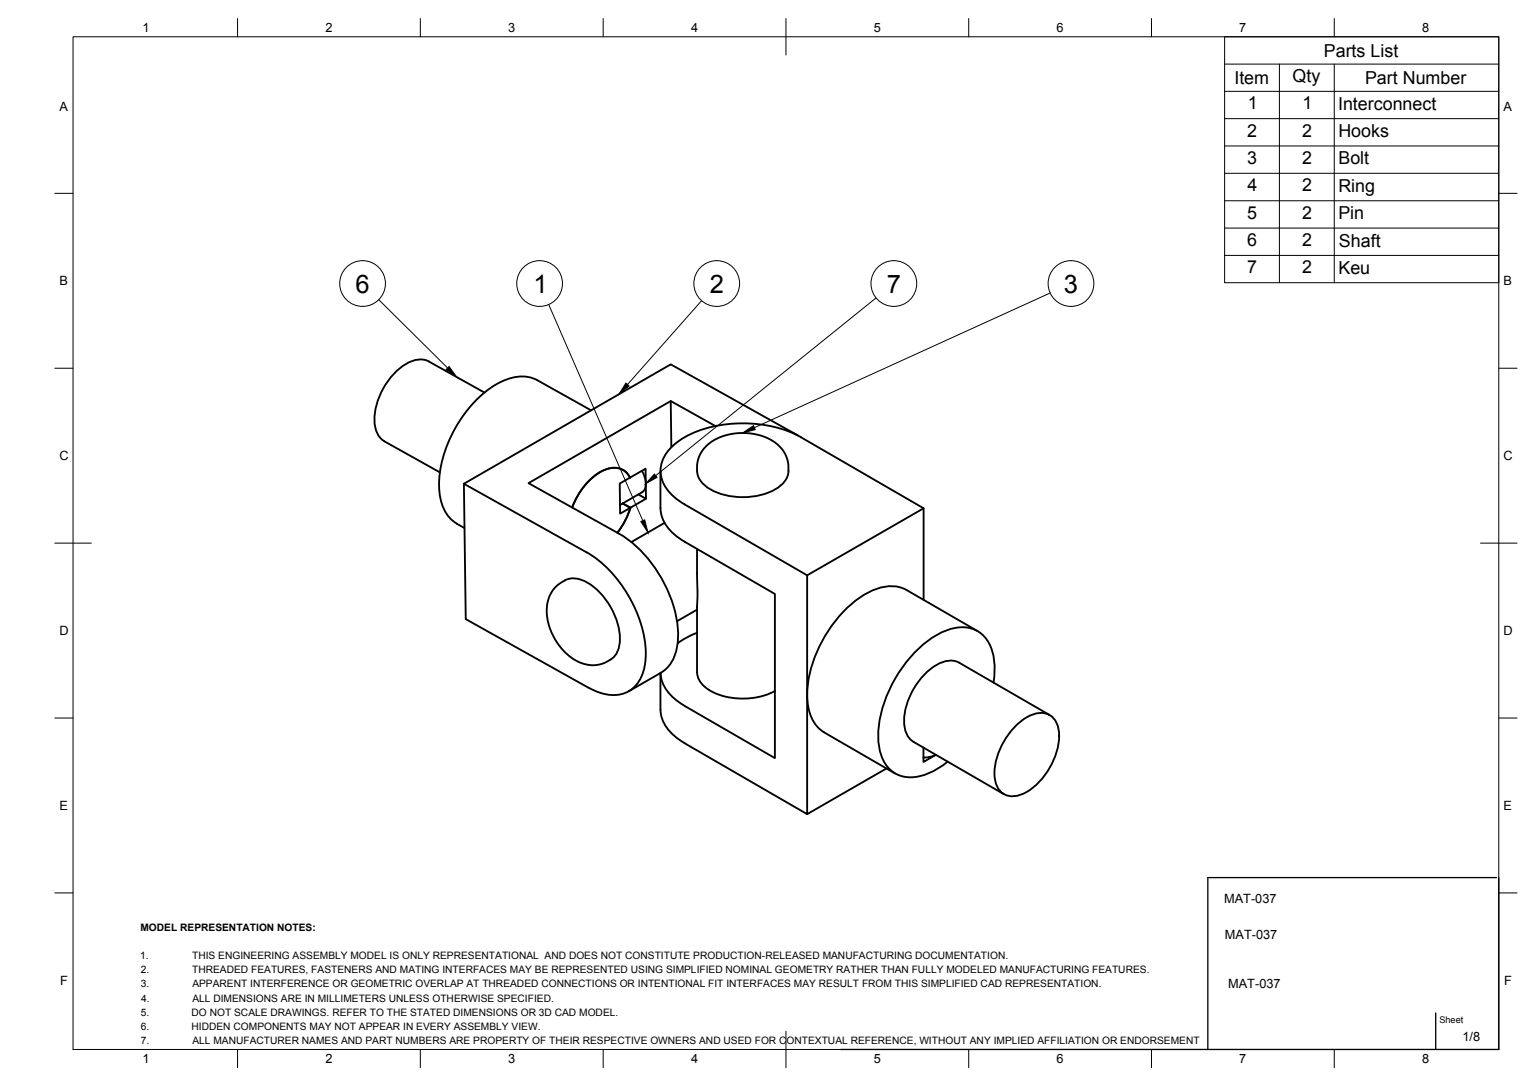
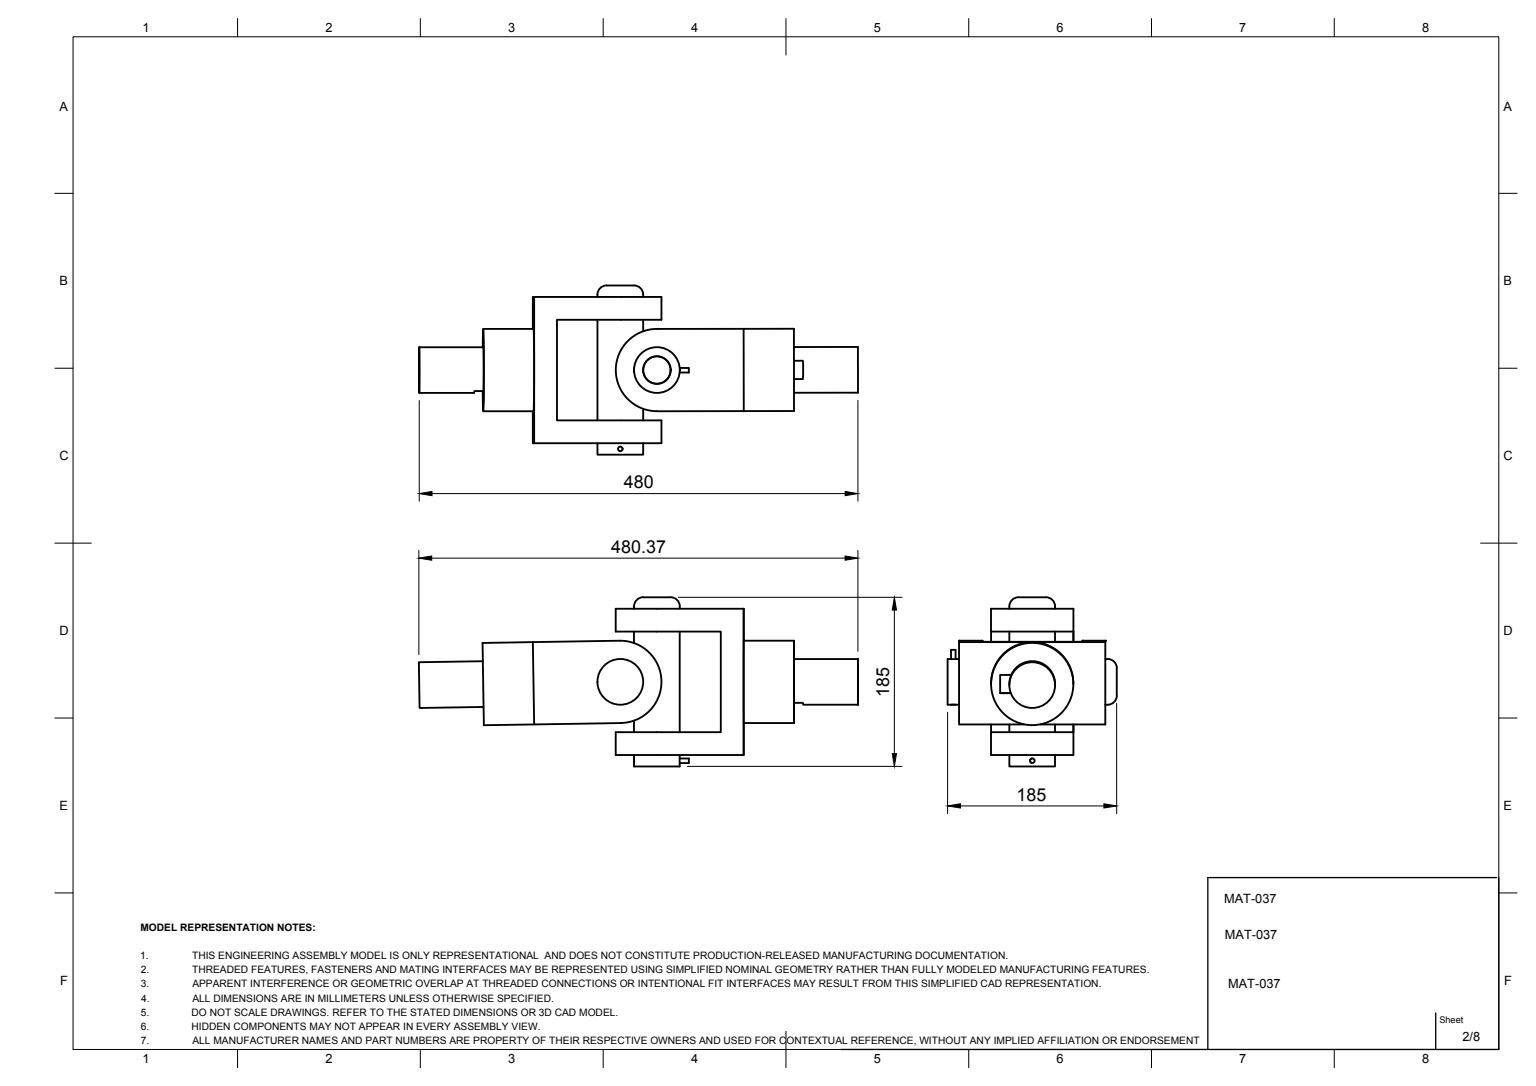
ISO-10303-21;
HEADER;
/* Generated by software containing ST-Developer
 * from STEP Tools, Inc. (www.steptools.com) 
 */

FILE_DESCRIPTION(
/* description */ ('STEP AP214'),
/* implementation_level */ '2;1');

FILE_NAME(
/* name */ 'MAT-037.step',
/* time_stamp */ '2026-11-14T21:09:07-08:00',
/* author */ (''),
/* organization */ (''),
/* preprocessor_version */ 'ST-DEVELOPER v20.2',
/* originating_system */ 'Autodesk Translation Framework v15.17.0.0',
/* authorisation */ '');

FILE_SCHEMA (('AUTOMOTIVE_DESIGN { 1 0 10303 214 3 1 1 }'));
ENDSEC;

DATA;
#10=MECHANICAL_DESIGN_GEOMETRIC_PRESENTATION_REPRESENTATION('',(#78,#79,
#80,#81,#82,#83,#84),#2059);
#11=ITEM_DEFINED_TRANSFORMATION($,$,#1061,#1167);
#12=ITEM_DEFINED_TRANSFORMATION($,$,#1078,#1168);
#13=ITEM_DEFINED_TRANSFORMATION($,$,#1111,#1169);
#14=ITEM_DEFINED_TRANSFORMATION($,$,#1126,#1170);
#15=ITEM_DEFINED_TRANSFORMATION($,$,#1137,#1171);
#16=ITEM_DEFINED_TRANSFORMATION($,$,#1143,#1172);
#17=ITEM_DEFINED_TRANSFORMATION($,$,#1156,#1173);
#18=ITEM_DEFINED_TRANSFORMATION($,$,#1078,#1174);
#19=ITEM_DEFINED_TRANSFORMATION($,$,#1111,#1175);
#20=ITEM_DEFINED_TRANSFORMATION($,$,#1126,#1176);
#21=ITEM_DEFINED_TRANSFORMATION($,$,#1137,#1177);
#22=ITEM_DEFINED_TRANSFORMATION($,$,#1143,#1178);
#23=ITEM_DEFINED_TRANSFORMATION($,$,#1156,#1179);
#24=(
REPRESENTATION_RELATIONSHIP($,$,#2094,#2093)
REPRESENTATION_RELATIONSHIP_WITH_TRANSFORMATION(#11)
SHAPE_REPRESENTATION_RELATIONSHIP()
);
#25=(
REPRESENTATION_RELATIONSHIP($,$,#2095,#2093)
REPRESENTATION_RELATIONSHIP_WITH_TRANSFORMATION(#12)
SHAPE_REPRESENTATION_RELATIONSHIP()
);
#26=(
REPRESENTATION_RELATIONSHIP($,$,#2096,#2093)
REPRESENTATION_RELATIONSHIP_WITH_TRANSFORMATION(#13)
SHAPE_REPRESENTATION_RELATIONSHIP()
);
#27=(
REPRESENTATION_RELATIONSHIP($,$,#2097,#2093)
REPRESENTATION_RELATIONSHIP_WITH_TRANSFORMATION(#14)
SHAPE_REPRESENTATION_RELATIONSHIP()
);
#28=(
REPRESENTATION_RELATIONSHIP($,$,#2098,#2093)
REPRESENTATION_RELATIONSHIP_WITH_TRANSFORMATION(#15)
SHAPE_REPRESENTATION_RELATIONSHIP()
);
#29=(
REPRESENTATION_RELATIONSHIP($,$,#2099,#2093)
REPRESENTATION_RELATIONSHIP_WITH_TRANSFORMATION(#16)
SHAPE_REPRESENTATION_RELATIONSHIP()
);
#30=(
REPRESENTATION_RELATIONSHIP($,$,#2100,#2093)
REPRESENTATION_RELATIONSHIP_WITH_TRANSFORMATION(#17)
SHAPE_REPRESENTATION_RELATIONSHIP()
);
#31=(
REPRESENTATION_RELATIONSHIP($,$,#2095,#2093)
REPRESENTATION_RELATIONSHIP_WITH_TRANSFORMATION(#18)
SHAPE_REPRESENTATION_RELATIONSHIP()
);
#32=(
REPRESENTATION_RELATIONSHIP($,$,#2096,#2093)
REPRESENTATION_RELATIONSHIP_WITH_TRANSFORMATION(#19)
SHAPE_REPRESENTATION_RELATIONSHIP()
);
#33=(
REPRESENTATION_RELATIONSHIP($,$,#2097,#2093)
REPRESENTATION_RELATIONSHIP_WITH_TRANSFORMATION(#20)
SHAPE_REPRESENTATION_RELATIONSHIP()
);
#34=(
REPRESENTATION_RELATIONSHIP($,$,#2098,#2093)
REPRESENTATION_RELATIONSHIP_WITH_TRANSFORMATION(#21)
SHAPE_REPRESENTATION_RELATIONSHIP()
);
#35=(
REPRESENTATION_RELATIONSHIP($,$,#2099,#2093)
REPRESENTATION_RELATIONSHIP_WITH_TRANSFORMATION(#22)
SHAPE_REPRESENTATION_RELATIONSHIP()
);
#36=(
REPRESENTATION_RELATIONSHIP($,$,#2100,#2093)
REPRESENTATION_RELATIONSHIP_WITH_TRANSFORMATION(#23)
SHAPE_REPRESENTATION_RELATIONSHIP()
);
#37=CONTEXT_DEPENDENT_SHAPE_REPRESENTATION(#24,#2080);
#38=CONTEXT_DEPENDENT_SHAPE_REPRESENTATION(#25,#2081);
#39=CONTEXT_DEPENDENT_SHAPE_REPRESENTATION(#26,#2082);
#40=CONTEXT_DEPENDENT_SHAPE_REPRESENTATION(#27,#2083);
#41=CONTEXT_DEPENDENT_SHAPE_REPRESENTATION(#28,#2084);
#42=CONTEXT_DEPENDENT_SHAPE_REPRESENTATION(#29,#2085);
#43=CONTEXT_DEPENDENT_SHAPE_REPRESENTATION(#30,#2086);
#44=CONTEXT_DEPENDENT_SHAPE_REPRESENTATION(#31,#2087);
#45=CONTEXT_DEPENDENT_SHAPE_REPRESENTATION(#32,#2088);
#46=CONTEXT_DEPENDENT_SHAPE_REPRESENTATION(#33,#2089);
#47=CONTEXT_DEPENDENT_SHAPE_REPRESENTATION(#34,#2090);
#48=CONTEXT_DEPENDENT_SHAPE_REPRESENTATION(#35,#2091);
#49=CONTEXT_DEPENDENT_SHAPE_REPRESENTATION(#36,#2092);
#50=NEXT_ASSEMBLY_USAGE_OCCURRENCE('interconnect:1','interconnect:1',
'interconnect:1',#2102,#2103,'interconnect:1');
#51=NEXT_ASSEMBLY_USAGE_OCCURRENCE('hooks:1','hooks:1','hooks:1',#2102,
#2104,'hooks:1');
#52=NEXT_ASSEMBLY_USAGE_OCCURRENCE('bolt:1','bolt:1','bolt:1',#2102,#2105,
'bolt:1');
#53=NEXT_ASSEMBLY_USAGE_OCCURRENCE('ring:1','ring:1','ring:1',#2102,#2106,
'ring:1');
#54=NEXT_ASSEMBLY_USAGE_OCCURRENCE('PIN:1','PIN:1','PIN:1',#2102,#2107,
'PIN:1');
#55=NEXT_ASSEMBLY_USAGE_OCCURRENCE('shaft:1','shaft:1','shaft:1',#2102,
#2108,'shaft:1');
#56=NEXT_ASSEMBLY_USAGE_OCCURRENCE('key:1','key:1','key:1',#2102,#2109,
'key:1');
#57=NEXT_ASSEMBLY_USAGE_OCCURRENCE('hooks:2','hooks:2','hooks:2',#2102,
#2104,'hooks:2');
#58=NEXT_ASSEMBLY_USAGE_OCCURRENCE('bolt:2','bolt:2','bolt:2',#2102,#2105,
'bolt:2');
#59=NEXT_ASSEMBLY_USAGE_OCCURRENCE('ring:2','ring:2','ring:2',#2102,#2106,
'ring:2');
#60=NEXT_ASSEMBLY_USAGE_OCCURRENCE('PIN:2','PIN:2','PIN:2',#2102,#2107,
'PIN:2');
#61=NEXT_ASSEMBLY_USAGE_OCCURRENCE('shaft:2','shaft:2','shaft:2',#2102,
#2108,'shaft:2');
#62=NEXT_ASSEMBLY_USAGE_OCCURRENCE('key:2','key:2','key:2',#2102,#2109,
'key:2');
#63=TOROIDAL_SURFACE('',#1112,15.,10.);
#64=SHAPE_REPRESENTATION_RELATIONSHIP('SRR','None',#2094,#71);
#65=SHAPE_REPRESENTATION_RELATIONSHIP('SRR','None',#2095,#72);
#66=SHAPE_REPRESENTATION_RELATIONSHIP('SRR','None',#2096,#73);
#67=SHAPE_REPRESENTATION_RELATIONSHIP('SRR','None',#2097,#74);
#68=SHAPE_REPRESENTATION_RELATIONSHIP('SRR','None',#2098,#75);
#69=SHAPE_REPRESENTATION_RELATIONSHIP('SRR','None',#2099,#76);
#70=SHAPE_REPRESENTATION_RELATIONSHIP('SRR','None',#2100,#77);
#71=ADVANCED_BREP_SHAPE_REPRESENTATION('',(#85),#2052);
#72=ADVANCED_BREP_SHAPE_REPRESENTATION('',(#86),#2053);
#73=ADVANCED_BREP_SHAPE_REPRESENTATION('',(#87),#2054);
#74=ADVANCED_BREP_SHAPE_REPRESENTATION('',(#88),#2055);
#75=ADVANCED_BREP_SHAPE_REPRESENTATION('',(#89),#2056);
#76=ADVANCED_BREP_SHAPE_REPRESENTATION('',(#90),#2057);
#77=ADVANCED_BREP_SHAPE_REPRESENTATION('',(#91),#2058);
#78=STYLED_ITEM('',(#2138),#85);
#79=STYLED_ITEM('',(#2139),#86);
#80=STYLED_ITEM('',(#2140),#87);
#81=STYLED_ITEM('',(#2141),#88);
#82=STYLED_ITEM('',(#2142),#89);
#83=STYLED_ITEM('',(#2142),#90);
#84=STYLED_ITEM('',(#2141),#91);
#85=MANIFOLD_SOLID_BREP('Body1',#975);
#86=MANIFOLD_SOLID_BREP('Body1',#976);
#87=MANIFOLD_SOLID_BREP('Body1',#977);
#88=MANIFOLD_SOLID_BREP('Body1',#978);
#89=MANIFOLD_SOLID_BREP('Body1',#979);
#90=MANIFOLD_SOLID_BREP('Body1',#980);
#91=MANIFOLD_SOLID_BREP('Body1',#981);
#92=PLANE('',#1074);
#93=PLANE('',#1075);
#94=PLANE('',#1076);
#95=PLANE('',#1077);
#96=PLANE('',#1092);
#97=PLANE('',#1093);
#98=PLANE('',#1094);
#99=PLANE('',#1095);
#100=PLANE('',#1097);
#101=PLANE('',#1098);
#102=PLANE('',#1100);
#103=PLANE('',#1102);
#104=PLANE('',#1103);
#105=PLANE('',#1105);
#106=PLANE('',#1108);
#107=PLANE('',#1109);
#108=PLANE('',#1110);
#109=PLANE('',#1123);
#110=PLANE('',#1124);
#111=PLANE('',#1125);
#112=PLANE('',#1135);
#113=PLANE('',#1136);
#114=PLANE('',#1141);
#115=PLANE('',#1142);
#116=PLANE('',#1148);
#117=PLANE('',#1149);
#118=PLANE('',#1150);
#119=PLANE('',#1152);
#120=PLANE('',#1154);
#121=PLANE('',#1157);
#122=PLANE('',#1158);
#123=PLANE('',#1161);
#124=PLANE('',#1162);
#125=FACE_BOUND('',#214,.T.);
#126=FACE_BOUND('',#217,.T.);
#127=FACE_BOUND('',#219,.T.);
#128=FACE_BOUND('',#221,.T.);
#129=FACE_BOUND('',#223,.T.);
#130=FACE_BOUND('',#225,.T.);
#131=FACE_BOUND('',#234,.T.);
#132=FACE_BOUND('',#237,.T.);
#133=FACE_BOUND('',#239,.T.);
#134=FACE_BOUND('',#241,.T.);
#135=FACE_BOUND('',#243,.T.);
#136=FACE_BOUND('',#245,.T.);
#137=FACE_BOUND('',#255,.T.);
#138=FACE_BOUND('',#258,.T.);
#139=FACE_BOUND('',#263,.T.);
#140=FACE_BOUND('',#264,.T.);
#141=FACE_BOUND('',#266,.T.);
#142=FACE_BOUND('',#267,.T.);
#143=FACE_BOUND('',#269,.T.);
#144=FACE_BOUND('',#271,.T.);
#145=B_SPLINE_CURVE_WITH_KNOTS('',3,(#1500,#1501,#1502,#1503,#1504,#1505,
#1506,#1507,#1508,#1509,#1510,#1511,#1512,#1513,#1514,#1515,#1516,#1517,
#1518,#1519,#1520,#1521,#1522,#1523,#1524,#1525,#1526,#1527,#1528,#1529,
#1530,#1531,#1532,#1533,#1534,#1535,#1536,#1537,#1538,#1539,#1540,#1541,
#1542,#1543,#1544,#1545,#1546,#1547,#1548,#1549,#1550,#1551,#1552,#1553,
#1554,#1555,#1556,#1557,#1558,#1559,#1560,#1561,#1562,#1563,#1564,#1565),
 .UNSPECIFIED.,.T.,.F.,(4,2,2,2,2,2,2,2,2,2,2,2,2,2,2,2,2,2,2,2,2,2,2,2,
2,2,2,2,2,2,2,2,4),(-13.1042885251054,-12.7312036729648,-12.3581188208242,
-11.9850339686836,-11.611949116543,-11.2858660599115,-10.95978300328,-10.3939996985545,
-9.82821639382906,-9.2624330891036,-8.69664978437814,-8.37056672774664,
-8.04448367111514,-7.67139881897453,-7.29831396683392,-6.92522911469332,
-6.55214426255271,-6.1790594104121,-5.80597455827149,-5.43288970613088,
-5.05980485399027,-4.73372179735877,-4.40763874072727,-3.84185543600181,
-3.27607213127635,-2.7102888265509,-2.14450552182544,-1.81842246519393,
-1.49233940856243,-1.11925455642182,-0.746169704281216,-0.373084852140608,
0.),.UNSPECIFIED.);
#146=B_SPLINE_CURVE_WITH_KNOTS('',3,(#1693,#1694,#1695,#1696,#1697,#1698,
#1699,#1700,#1701,#1702,#1703,#1704,#1705,#1706,#1707,#1708,#1709,#1710),
 .UNSPECIFIED.,.F.,.F.,(4,2,2,2,2,2,2,2,4),(0.377444585314899,0.471804471485951,
0.566164357657003,0.660526764143401,0.754889170629798,0.849251577116196,
0.943613983602594,1.03797386977365,1.1323337559447),.UNSPECIFIED.);
#147=B_SPLINE_CURVE_WITH_KNOTS('',3,(#1713,#1714,#1715,#1716,#1717,#1718,
#1719,#1720,#1721,#1722,#1723,#1724,#1725,#1726,#1727,#1728,#1729,#1730,
#1731,#1732,#1733,#1734,#1735,#1736,#1737,#1738,#1739,#1740,#1741,#1742,
#1743,#1744,#1745,#1746),.UNSPECIFIED.,.T.,.F.,(4,2,2,2,2,2,2,2,2,2,2,2,
2,2,2,2,4),(-1.5097783412596,-1.4154159347732,-1.3210535282868,-1.22669364211575,
-1.1323337559447,-1.03797386977365,-0.943613983602594,-0.849251577116196,
-0.754889170629798,-0.660526764143401,-0.566164357657003,-0.471804471485951,
-0.377444585314899,-0.283084699143847,-0.188724812972796,-0.0943624064863978,
0.),.UNSPECIFIED.);
#148=B_SPLINE_CURVE_WITH_KNOTS('',3,(#1747,#1748,#1749,#1750,#1751,#1752,
#1753,#1754,#1755,#1756,#1757,#1758,#1759,#1760,#1761,#1762,#1763,#1764,
#1765),.UNSPECIFIED.,.F.,.F.,(4,2,2,2,3,2,2,2,4),(1.1323337559447,1.22669364211575,
1.3210535282868,1.4154159347732,1.5097783412596,1.60414074774599,1.69850315423239,
1.79286304040344,1.8872229265745),.UNSPECIFIED.);
#149=B_SPLINE_CURVE_WITH_KNOTS('',3,(#1783,#1784,#1785,#1786,#1787,#1788,
#1789,#1790,#1791,#1792,#1793,#1794,#1795,#1796,#1797,#1798,#1799,#1800,
#1801,#1802,#1803,#1804,#1805,#1806,#1807,#1808,#1809,#1810,#1811,#1812,
#1813,#1814,#1815,#1816),.UNSPECIFIED.,.T.,.F.,(4,2,2,2,2,2,2,2,2,2,2,2,
2,2,2,2,4),(0.,0.0942394555075742,0.188478911015148,0.28271804575446,0.376957180493772,
0.471196315233084,0.565435449972396,0.65967490547997,0.753914360987544,
0.848153816495118,0.942393272002692,1.036632406742,1.13087154148132,1.22511067622063,
1.31934981095994,1.41358926646751,1.50782872197509),.UNSPECIFIED.);
#150=B_SPLINE_CURVE_WITH_KNOTS('',3,(#1820,#1821,#1822,#1823,#1824,#1825,
#1826,#1827,#1828,#1829,#1830,#1831,#1832,#1833,#1834,#1835,#1836,#1837),
 .UNSPECIFIED.,.F.,.F.,(4,2,2,2,2,2,2,2,4),(0.377444585314897,0.471804471485949,
0.566164357657001,0.660526764143398,0.754889170629794,0.849251577116191,
0.943613983602588,1.03797386977364,1.13233375594469),.UNSPECIFIED.);
#151=B_SPLINE_CURVE_WITH_KNOTS('',3,(#1838,#1839,#1840,#1841,#1842,#1843,
#1844,#1845,#1846,#1847,#1848,#1849,#1850,#1851,#1852,#1853,#1854,#1855,
#1856),.UNSPECIFIED.,.F.,.F.,(4,2,2,2,3,2,2,2,4),(-0.377444585314897,-0.283084699143845,
-0.188724812972793,-0.0943624064863967,0.,0.0943624064863968,0.188724812972794,
0.283084699143845,0.377444585314897),.UNSPECIFIED.);
#152=B_SPLINE_CURVE_WITH_KNOTS('',3,(#1860,#1861,#1862,#1863,#1864,#1865,
#1866,#1867,#1868,#1869,#1870,#1871,#1872,#1873,#1874,#1875,#1876,#1877),
 .UNSPECIFIED.,.F.,.F.,(4,2,2,2,2,2,2,2,4),(0.377444585314897,0.471804471485949,
0.566164357657001,0.660526764143397,0.754889170629794,0.849251577116191,
0.943613983602588,1.03797386977364,1.13233375594469),.UNSPECIFIED.);
#153=B_SPLINE_CURVE_WITH_KNOTS('',3,(#1880,#1881,#1882,#1883,#1884,#1885,
#1886,#1887,#1888,#1889,#1890,#1891,#1892,#1893,#1894,#1895,#1896,#1897,
#1898,#1899,#1900,#1901,#1902,#1903,#1904,#1905,#1906,#1907,#1908,#1909,
#1910,#1911,#1912,#1913),.UNSPECIFIED.,.T.,.F.,(4,2,2,2,2,2,2,2,2,2,2,2,
2,2,2,2,4),(-1.50782872197509,-1.41358926646751,-1.31934981095994,-1.22511067622063,
-1.13087154148132,-1.036632406742,-0.942393272002692,-0.848153816495118,
-0.753914360987544,-0.65967490547997,-0.565435449972396,-0.471196315233084,
-0.376957180493772,-0.28271804575446,-0.188478911015148,-0.0942394555075742,
0.),.UNSPECIFIED.);
#154=B_SPLINE_CURVE_WITH_KNOTS('',3,(#1914,#1915,#1916,#1917,#1918,#1919,
#1920,#1921,#1922,#1923,#1924,#1925,#1926,#1927,#1928,#1929,#1930,#1931,
#1932),.UNSPECIFIED.,.F.,.F.,(4,2,2,2,3,2,2,2,4),(1.13233375594469,1.22669364211574,
1.32105352828679,1.41541593477319,1.50977834125959,1.60414074774598,1.69850315423238,
1.79286304040343,1.88722292657449),.UNSPECIFIED.);
#155=B_SPLINE_CURVE_WITH_KNOTS('',3,(#1969,#1970,#1971,#1972,#1973,#1974,
#1975,#1976,#1977,#1978,#1979,#1980,#1981,#1982),.UNSPECIFIED.,.F.,.F.,
(4,2,2,2,2,2,4),(-3.67157631505784,-3.33396300865433,-3.01698728047981,
-2.7000115523053,-2.38303582413079,-2.06606009595627,-1.72844678955265),
 .UNSPECIFIED.);
#156=FACE_OUTER_BOUND('',#212,.T.);
#157=FACE_OUTER_BOUND('',#213,.T.);
#158=FACE_OUTER_BOUND('',#215,.T.);
#159=FACE_OUTER_BOUND('',#216,.T.);
#160=FACE_OUTER_BOUND('',#218,.T.);
#161=FACE_OUTER_BOUND('',#220,.T.);
#162=FACE_OUTER_BOUND('',#222,.T.);
#163=FACE_OUTER_BOUND('',#224,.T.);
#164=FACE_OUTER_BOUND('',#226,.T.);
#165=FACE_OUTER_BOUND('',#227,.T.);
#166=FACE_OUTER_BOUND('',#228,.T.);
#167=FACE_OUTER_BOUND('',#229,.T.);
#168=FACE_OUTER_BOUND('',#230,.T.);
#169=FACE_OUTER_BOUND('',#231,.T.);
#170=FACE_OUTER_BOUND('',#232,.T.);
#171=FACE_OUTER_BOUND('',#233,.T.);
#172=FACE_OUTER_BOUND('',#235,.T.);
#173=FACE_OUTER_BOUND('',#236,.T.);
#174=FACE_OUTER_BOUND('',#238,.T.);
#175=FACE_OUTER_BOUND('',#240,.T.);
#176=FACE_OUTER_BOUND('',#242,.T.);
#177=FACE_OUTER_BOUND('',#244,.T.);
#178=FACE_OUTER_BOUND('',#246,.T.);
#179=FACE_OUTER_BOUND('',#247,.T.);
#180=FACE_OUTER_BOUND('',#248,.T.);
#181=FACE_OUTER_BOUND('',#249,.T.);
#182=FACE_OUTER_BOUND('',#250,.T.);
#183=FACE_OUTER_BOUND('',#251,.T.);
#184=FACE_OUTER_BOUND('',#252,.T.);
#185=FACE_OUTER_BOUND('',#253,.T.);
#186=FACE_OUTER_BOUND('',#254,.T.);
#187=FACE_OUTER_BOUND('',#256,.T.);
#188=FACE_OUTER_BOUND('',#257,.T.);
#189=FACE_OUTER_BOUND('',#259,.T.);
#190=FACE_OUTER_BOUND('',#260,.T.);
#191=FACE_OUTER_BOUND('',#261,.T.);
#192=FACE_OUTER_BOUND('',#262,.T.);
#193=FACE_OUTER_BOUND('',#265,.T.);
#194=FACE_OUTER_BOUND('',#268,.T.);
#195=FACE_OUTER_BOUND('',#270,.T.);
#196=FACE_OUTER_BOUND('',#272,.T.);
#197=FACE_OUTER_BOUND('',#273,.T.);
#198=FACE_OUTER_BOUND('',#274,.T.);
#199=FACE_OUTER_BOUND('',#275,.T.);
#200=FACE_OUTER_BOUND('',#276,.T.);
#201=FACE_OUTER_BOUND('',#277,.T.);
#202=FACE_OUTER_BOUND('',#278,.T.);
#203=FACE_OUTER_BOUND('',#279,.T.);
#204=FACE_OUTER_BOUND('',#280,.T.);
#205=FACE_OUTER_BOUND('',#281,.T.);
#206=FACE_OUTER_BOUND('',#282,.T.);
#207=FACE_OUTER_BOUND('',#283,.T.);
#208=FACE_OUTER_BOUND('',#284,.T.);
#209=FACE_OUTER_BOUND('',#285,.T.);
#210=FACE_OUTER_BOUND('',#286,.T.);
#211=FACE_OUTER_BOUND('',#287,.T.);
#212=EDGE_LOOP('',(#659,#660,#661,#662));
#213=EDGE_LOOP('',(#663,#664,#665,#666));
#214=EDGE_LOOP('',(#667));
#215=EDGE_LOOP('',(#668,#669,#670,#671));
#216=EDGE_LOOP('',(#672,#673,#674,#675));
#217=EDGE_LOOP('',(#676));
#218=EDGE_LOOP('',(#677));
#219=EDGE_LOOP('',(#678));
#220=EDGE_LOOP('',(#679));
#221=EDGE_LOOP('',(#680));
#222=EDGE_LOOP('',(#681));
#223=EDGE_LOOP('',(#682));
#224=EDGE_LOOP('',(#683));
#225=EDGE_LOOP('',(#684));
#226=EDGE_LOOP('',(#685,#686,#687,#688));
#227=EDGE_LOOP('',(#689,#690,#691,#692));
#228=EDGE_LOOP('',(#693,#694,#695,#696));
#229=EDGE_LOOP('',(#697,#698,#699,#700,#701));
#230=EDGE_LOOP('',(#702,#703,#704,#705,#706,#707,#708,#709,#710));
#231=EDGE_LOOP('',(#711,#712,#713,#714,#715,#716,#717,#718,#719));
#232=EDGE_LOOP('',(#720,#721,#722,#723));
#233=EDGE_LOOP('',(#724,#725,#726,#727));
#234=EDGE_LOOP('',(#728));
#235=EDGE_LOOP('',(#729,#730,#731,#732));
#236=EDGE_LOOP('',(#733,#734,#735,#736));
#237=EDGE_LOOP('',(#737));
#238=EDGE_LOOP('',(#738,#739,#740,#741));
#239=EDGE_LOOP('',(#742));
#240=EDGE_LOOP('',(#743,#744,#745,#746));
#241=EDGE_LOOP('',(#747,#748,#749,#750));
#242=EDGE_LOOP('',(#751,#752,#753,#754));
#243=EDGE_LOOP('',(#755));
#244=EDGE_LOOP('',(#756));
#245=EDGE_LOOP('',(#757,#758,#759,#760));
#246=EDGE_LOOP('',(#761,#762,#763,#764));
#247=EDGE_LOOP('',(#765,#766,#767,#768));
#248=EDGE_LOOP('',(#769,#770,#771,#772));
#249=EDGE_LOOP('',(#773,#774,#775,#776));
#250=EDGE_LOOP('',(#777,#778,#779,#780));
#251=EDGE_LOOP('',(#781,#782,#783,#784,#785));
#252=EDGE_LOOP('',(#786,#787,#788,#789,#790));
#253=EDGE_LOOP('',(#791,#792,#793,#794,#795));
#254=EDGE_LOOP('',(#796,#797,#798,#799,#800,#801,#802,#803));
#255=EDGE_LOOP('',(#804));
#256=EDGE_LOOP('',(#805));
#257=EDGE_LOOP('',(#806));
#258=EDGE_LOOP('',(#807));
#259=EDGE_LOOP('',(#808));
#260=EDGE_LOOP('',(#809,#810,#811,#812,#813));
#261=EDGE_LOOP('',(#814,#815,#816,#817,#818));
#262=EDGE_LOOP('',(#819,#820,#821,#822));
#263=EDGE_LOOP('',(#823,#824));
#264=EDGE_LOOP('',(#825,#826));
#265=EDGE_LOOP('',(#827,#828,#829,#830));
#266=EDGE_LOOP('',(#831));
#267=EDGE_LOOP('',(#832));
#268=EDGE_LOOP('',(#833));
#269=EDGE_LOOP('',(#834));
#270=EDGE_LOOP('',(#835));
#271=EDGE_LOOP('',(#836));
#272=EDGE_LOOP('',(#837,#838,#839,#840));
#273=EDGE_LOOP('',(#841));
#274=EDGE_LOOP('',(#842));
#275=EDGE_LOOP('',(#843,#844,#845,#846,#847,#848,#849,#850));
#276=EDGE_LOOP('',(#851,#852,#853,#854,#855));
#277=EDGE_LOOP('',(#856));
#278=EDGE_LOOP('',(#857,#858,#859,#860));
#279=EDGE_LOOP('',(#861,#862,#863,#864));
#280=EDGE_LOOP('',(#865,#866,#867,#868));
#281=EDGE_LOOP('',(#869,#870,#871,#872));
#282=EDGE_LOOP('',(#873,#874,#875,#876));
#283=EDGE_LOOP('',(#877,#878,#879,#880));
#284=EDGE_LOOP('',(#881,#882,#883,#884));
#285=EDGE_LOOP('',(#885,#886,#887,#888));
#286=EDGE_LOOP('',(#889,#890,#891,#892));
#287=EDGE_LOOP('',(#893,#894,#895,#896));
#288=LINE('',#1491,#353);
#289=LINE('',#1497,#354);
#290=LINE('',#1570,#355);
#291=LINE('',#1576,#356);
#292=LINE('',#1587,#357);
#293=LINE('',#1593,#358);
#294=LINE('',#1600,#359);
#295=LINE('',#1603,#360);
#296=LINE('',#1609,#361);
#297=LINE('',#1615,#362);
#298=LINE('',#1617,#363);
#299=LINE('',#1619,#364);
#300=LINE('',#1621,#365);
#301=LINE('',#1623,#366);
#302=LINE('',#1625,#367);
#303=LINE('',#1627,#368);
#304=LINE('',#1628,#369);
#305=LINE('',#1629,#370);
#306=LINE('',#1633,#371);
#307=LINE('',#1635,#372);
#308=LINE('',#1636,#373);
#309=LINE('',#1638,#374);
#310=LINE('',#1640,#375);
#311=LINE('',#1642,#376);
#312=LINE('',#1644,#377);
#313=LINE('',#1646,#378);
#314=LINE('',#1647,#379);
#315=LINE('',#1649,#380);
#316=LINE('',#1653,#381);
#317=LINE('',#1658,#382);
#318=LINE('',#1660,#383);
#319=LINE('',#1662,#384);
#320=LINE('',#1664,#385);
#321=LINE('',#1665,#386);
#322=LINE('',#1670,#387);
#323=LINE('',#1672,#388);
#324=LINE('',#1673,#389);
#325=LINE('',#1677,#390);
#326=LINE('',#1679,#391);
#327=LINE('',#1712,#392);
#328=LINE('',#1769,#393);
#329=LINE('',#1773,#394);
#330=LINE('',#1775,#395);
#331=LINE('',#1818,#396);
#332=LINE('',#1879,#397);
#333=LINE('',#1937,#398);
#334=LINE('',#1943,#399);
#335=LINE('',#1952,#400);
#336=LINE('',#1962,#401);
#337=LINE('',#1967,#402);
#338=LINE('',#1983,#403);
#339=LINE('',#1986,#404);
#340=LINE('',#1988,#405);
#341=LINE('',#1989,#406);
#342=LINE('',#1994,#407);
#343=LINE('',#1997,#408);
#344=LINE('',#2000,#409);
#345=LINE('',#2006,#410);
#346=LINE('',#2008,#411);
#347=LINE('',#2010,#412);
#348=LINE('',#2011,#413);
#349=LINE('',#2016,#414);
#350=LINE('',#2020,#415);
#351=LINE('',#2022,#416);
#352=LINE('',#2023,#417);
#353=VECTOR('',#1188,15.);
#354=VECTOR('',#1195,25.);
#355=VECTOR('',#1202,15.);
#356=VECTOR('',#1209,25.);
#357=VECTOR('',#1226,15.0000000000001);
#358=VECTOR('',#1233,15.0000000000001);
#359=VECTOR('',#1240,1000.);
#360=VECTOR('',#1243,1000.);
#361=VECTOR('',#1248,45.0000000000003);
#362=VECTOR('',#1255,1000.);
#363=VECTOR('',#1256,1000.);
#364=VECTOR('',#1257,1000.);
#365=VECTOR('',#1258,1000.);
#366=VECTOR('',#1259,1000.);
#367=VECTOR('',#1260,1000.);
#368=VECTOR('',#1261,1000.);
#369=VECTOR('',#1262,1000.);
#370=VECTOR('',#1263,1000.);
#371=VECTOR('',#1266,1000.);
#372=VECTOR('',#1267,1000.);
#373=VECTOR('',#1268,1000.);
#374=VECTOR('',#1269,1000.);
#375=VECTOR('',#1270,1000.);
#376=VECTOR('',#1271,1000.);
#377=VECTOR('',#1272,1000.);
#378=VECTOR('',#1273,1000.);
#379=VECTOR('',#1274,1000.);
#380=VECTOR('',#1277,1000.);
#381=VECTOR('',#1284,1000.);
#382=VECTOR('',#1293,1000.);
#383=VECTOR('',#1296,1000.);
#384=VECTOR('',#1297,1000.);
#385=VECTOR('',#1298,1000.);
#386=VECTOR('',#1299,1000.);
#387=VECTOR('',#1306,1000.);
#388=VECTOR('',#1307,1000.);
#389=VECTOR('',#1308,1000.);
#390=VECTOR('',#1315,1000.);
#391=VECTOR('',#1318,1000.);
#392=VECTOR('',#1335,2.5);
#393=VECTOR('',#1340,25.);
#394=VECTOR('',#1345,15.);
#395=VECTOR('',#1346,15.);
#396=VECTOR('',#1359,2.49999999999999);
#397=VECTOR('',#1362,2.49999999999999);
#398=VECTOR('',#1367,15.);
#399=VECTOR('',#1374,25.);
#400=VECTOR('',#1387,2.49999999999999);
#401=VECTOR('',#1400,25.0000000000002);
#402=VECTOR('',#1405,1000.);
#403=VECTOR('',#1406,1000.);
#404=VECTOR('',#1409,1000.);
#405=VECTOR('',#1410,1000.);
#406=VECTOR('',#1411,1000.);
#407=VECTOR('',#1418,1000.);
#408=VECTOR('',#1421,1000.);
#409=VECTOR('',#1426,1000.);
#410=VECTOR('',#1433,1000.);
#411=VECTOR('',#1434,1000.);
#412=VECTOR('',#1435,1000.);
#413=VECTOR('',#1436,1000.);
#414=VECTOR('',#1441,1000.);
#415=VECTOR('',#1446,1000.);
#416=VECTOR('',#1447,1000.);
#417=VECTOR('',#1448,1000.);
#418=CIRCLE('',#1063,15.);
#419=CIRCLE('',#1064,15.);
#420=CIRCLE('',#1066,25.);
#421=CIRCLE('',#1067,25.);
#422=CIRCLE('',#1069,15.);
#423=CIRCLE('',#1070,15.);
#424=CIRCLE('',#1072,25.);
#425=CIRCLE('',#1073,25.);
#426=CIRCLE('',#1080,15.0000000000001);
#427=CIRCLE('',#1081,15.0000000000001);
#428=CIRCLE('',#1083,15.0000000000001);
#429=CIRCLE('',#1084,15.0000000000001);
#430=CIRCLE('',#1086,25.0000000000002);
#431=CIRCLE('',#1087,25.0000000000002);
#432=CIRCLE('',#1089,45.0000000000003);
#433=CIRCLE('',#1090,45.0000000000003);
#434=CIRCLE('',#1091,45.0000000000003);
#435=CIRCLE('',#1096,45.0000000000003);
#436=CIRCLE('',#1099,45.0000000000003);
#437=CIRCLE('',#1101,45.0000000000003);
#438=CIRCLE('',#1104,45.0000000000003);
#439=CIRCLE('',#1113,15.);
#440=CIRCLE('',#1114,10.);
#441=CIRCLE('',#1115,25.);
#442=CIRCLE('',#1116,25.);
#443=CIRCLE('',#1119,25.);
#444=CIRCLE('',#1121,15.);
#445=CIRCLE('',#1122,15.);
#446=CIRCLE('',#1130,15.);
#447=CIRCLE('',#1131,15.);
#448=CIRCLE('',#1133,25.);
#449=CIRCLE('',#1134,25.);
#450=CIRCLE('',#1139,2.49999999999999);
#451=CIRCLE('',#1140,2.49999999999999);
#452=CIRCLE('',#1145,25.0000000000002);
#453=CIRCLE('',#1146,25.0000000000002);
#454=CIRCLE('',#1147,25.0000000000002);
#455=CIRCLE('',#1151,10.0000000000001);
#456=CIRCLE('',#1153,10.0000000000001);
#457=CIRCLE('',#1159,10.0000000000001);
#458=CIRCLE('',#1160,10.0000000000001);
#459=CIRCLE('',#1163,10.0000000000001);
#460=CIRCLE('',#1164,10.0000000000001);
#461=VERTEX_POINT('',#1488);
#462=VERTEX_POINT('',#1490);
#463=VERTEX_POINT('',#1494);
#464=VERTEX_POINT('',#1496);
#465=VERTEX_POINT('',#1499);
#466=VERTEX_POINT('',#1567);
#467=VERTEX_POINT('',#1569);
#468=VERTEX_POINT('',#1573);
#469=VERTEX_POINT('',#1575);
#470=VERTEX_POINT('',#1584);
#471=VERTEX_POINT('',#1586);
#472=VERTEX_POINT('',#1590);
#473=VERTEX_POINT('',#1592);
#474=VERTEX_POINT('',#1596);
#475=VERTEX_POINT('',#1597);
#476=VERTEX_POINT('',#1599);
#477=VERTEX_POINT('',#1601);
#478=VERTEX_POINT('',#1605);
#479=VERTEX_POINT('',#1606);
#480=VERTEX_POINT('',#1608);
#481=VERTEX_POINT('',#1613);
#482=VERTEX_POINT('',#1614);
#483=VERTEX_POINT('',#1616);
#484=VERTEX_POINT('',#1618);
#485=VERTEX_POINT('',#1620);
#486=VERTEX_POINT('',#1622);
#487=VERTEX_POINT('',#1624);
#488=VERTEX_POINT('',#1626);
#489=VERTEX_POINT('',#1631);
#490=VERTEX_POINT('',#1632);
#491=VERTEX_POINT('',#1634);
#492=VERTEX_POINT('',#1637);
#493=VERTEX_POINT('',#1639);
#494=VERTEX_POINT('',#1641);
#495=VERTEX_POINT('',#1643);
#496=VERTEX_POINT('',#1645);
#497=VERTEX_POINT('',#1661);
#498=VERTEX_POINT('',#1663);
#499=VERTEX_POINT('',#1669);
#500=VERTEX_POINT('',#1671);
#501=VERTEX_POINT('',#1683);
#502=VERTEX_POINT('',#1685);
#503=VERTEX_POINT('',#1687);
#504=VERTEX_POINT('',#1691);
#505=VERTEX_POINT('',#1692);
#506=VERTEX_POINT('',#1711);
#507=VERTEX_POINT('',#1767);
#508=VERTEX_POINT('',#1771);
#509=VERTEX_POINT('',#1774);
#510=VERTEX_POINT('',#1782);
#511=VERTEX_POINT('',#1817);
#512=VERTEX_POINT('',#1819);
#513=VERTEX_POINT('',#1858);
#514=VERTEX_POINT('',#1859);
#515=VERTEX_POINT('',#1878);
#516=VERTEX_POINT('',#1934);
#517=VERTEX_POINT('',#1936);
#518=VERTEX_POINT('',#1940);
#519=VERTEX_POINT('',#1942);
#520=VERTEX_POINT('',#1949);
#521=VERTEX_POINT('',#1951);
#522=VERTEX_POINT('',#1958);
#523=VERTEX_POINT('',#1959);
#524=VERTEX_POINT('',#1961);
#525=VERTEX_POINT('',#1964);
#526=VERTEX_POINT('',#1966);
#527=VERTEX_POINT('',#1968);
#528=VERTEX_POINT('',#1985);
#529=VERTEX_POINT('',#1987);
#530=VERTEX_POINT('',#1992);
#531=VERTEX_POINT('',#1996);
#532=VERTEX_POINT('',#2004);
#533=VERTEX_POINT('',#2005);
#534=VERTEX_POINT('',#2007);
#535=VERTEX_POINT('',#2009);
#536=VERTEX_POINT('',#2013);
#537=VERTEX_POINT('',#2015);
#538=VERTEX_POINT('',#2019);
#539=VERTEX_POINT('',#2021);
#540=EDGE_CURVE('',#461,#461,#418,.T.);
#541=EDGE_CURVE('',#461,#462,#288,.T.);
#542=EDGE_CURVE('',#462,#462,#419,.T.);
#543=EDGE_CURVE('',#463,#463,#420,.T.);
#544=EDGE_CURVE('',#463,#464,#289,.T.);
#545=EDGE_CURVE('',#464,#464,#421,.T.);
#546=EDGE_CURVE('',#465,#465,#145,.T.);
#547=EDGE_CURVE('',#466,#466,#422,.T.);
#548=EDGE_CURVE('',#466,#467,#290,.T.);
#549=EDGE_CURVE('',#467,#467,#423,.T.);
#550=EDGE_CURVE('',#468,#468,#424,.T.);
#551=EDGE_CURVE('',#468,#469,#291,.T.);
#552=EDGE_CURVE('',#469,#469,#425,.T.);
#553=EDGE_CURVE('',#470,#470,#426,.T.);
#554=EDGE_CURVE('',#470,#471,#292,.T.);
#555=EDGE_CURVE('',#471,#471,#427,.T.);
#556=EDGE_CURVE('',#472,#472,#428,.T.);
#557=EDGE_CURVE('',#472,#473,#293,.T.);
#558=EDGE_CURVE('',#473,#473,#429,.T.);
#559=EDGE_CURVE('',#474,#475,#430,.T.);
#560=EDGE_CURVE('',#476,#474,#294,.T.);
#561=EDGE_CURVE('',#476,#477,#431,.T.);
#562=EDGE_CURVE('',#475,#477,#295,.T.);
#563=EDGE_CURVE('',#478,#479,#432,.T.);
#564=EDGE_CURVE('',#478,#480,#296,.T.);
#565=EDGE_CURVE('',#480,#480,#433,.T.);
#566=EDGE_CURVE('',#479,#478,#434,.T.);
#567=EDGE_CURVE('',#481,#482,#297,.T.);
#568=EDGE_CURVE('',#482,#483,#298,.T.);
#569=EDGE_CURVE('',#483,#484,#299,.T.);
#570=EDGE_CURVE('',#485,#484,#300,.T.);
#571=EDGE_CURVE('',#485,#486,#301,.T.);
#572=EDGE_CURVE('',#486,#487,#302,.T.);
#573=EDGE_CURVE('',#487,#488,#303,.T.);
#574=EDGE_CURVE('',#488,#478,#304,.T.);
#575=EDGE_CURVE('',#478,#481,#305,.T.);
#576=EDGE_CURVE('',#489,#490,#306,.T.);
#577=EDGE_CURVE('',#491,#489,#307,.T.);
#578=EDGE_CURVE('',#479,#491,#308,.T.);
#579=EDGE_CURVE('',#492,#479,#309,.T.);
#580=EDGE_CURVE('',#493,#492,#310,.T.);
#581=EDGE_CURVE('',#494,#493,#311,.T.);
#582=EDGE_CURVE('',#495,#494,#312,.T.);
#583=EDGE_CURVE('',#495,#496,#313,.T.);
#584=EDGE_CURVE('',#490,#496,#314,.T.);
#585=EDGE_CURVE('',#488,#492,#315,.T.);
#586=EDGE_CURVE('',#493,#487,#435,.T.);
#587=EDGE_CURVE('',#481,#491,#316,.T.);
#588=EDGE_CURVE('',#489,#482,#436,.T.);
#589=EDGE_CURVE('',#483,#490,#437,.T.);
#590=EDGE_CURVE('',#484,#496,#317,.T.);
#591=EDGE_CURVE('',#485,#495,#318,.T.);
#592=EDGE_CURVE('',#477,#497,#319,.T.);
#593=EDGE_CURVE('',#498,#476,#320,.T.);
#594=EDGE_CURVE('',#497,#498,#321,.T.);
#595=EDGE_CURVE('',#494,#486,#438,.T.);
#596=EDGE_CURVE('',#499,#475,#322,.T.);
#597=EDGE_CURVE('',#500,#499,#323,.T.);
#598=EDGE_CURVE('',#474,#500,#324,.T.);
#599=EDGE_CURVE('',#497,#499,#325,.T.);
#600=EDGE_CURVE('',#498,#500,#326,.T.);
#601=EDGE_CURVE('',#501,#501,#439,.T.);
#602=EDGE_CURVE('',#501,#502,#440,.T.);
#603=EDGE_CURVE('',#503,#502,#441,.T.);
#604=EDGE_CURVE('',#502,#503,#442,.T.);
#605=EDGE_CURVE('',#504,#505,#146,.T.);
#606=EDGE_CURVE('',#504,#506,#327,.T.);
#607=EDGE_CURVE('',#506,#506,#147,.T.);
#608=EDGE_CURVE('',#505,#504,#148,.T.);
#609=EDGE_CURVE('',#507,#507,#443,.T.);
#610=EDGE_CURVE('',#507,#503,#328,.T.);
#611=EDGE_CURVE('',#508,#508,#444,.T.);
#612=EDGE_CURVE('',#508,#504,#329,.T.);
#613=EDGE_CURVE('',#505,#509,#330,.T.);
#614=EDGE_CURVE('',#509,#509,#445,.T.);
#615=EDGE_CURVE('',#510,#510,#149,.T.);
#616=EDGE_CURVE('',#510,#511,#331,.T.);
#617=EDGE_CURVE('',#511,#512,#150,.T.);
#618=EDGE_CURVE('',#512,#511,#151,.T.);
#619=EDGE_CURVE('',#513,#514,#152,.T.);
#620=EDGE_CURVE('',#514,#515,#332,.T.);
#621=EDGE_CURVE('',#515,#515,#153,.T.);
#622=EDGE_CURVE('',#514,#513,#154,.T.);
#623=EDGE_CURVE('',#516,#516,#446,.T.);
#624=EDGE_CURVE('',#516,#517,#333,.T.);
#625=EDGE_CURVE('',#517,#517,#447,.T.);
#626=EDGE_CURVE('',#518,#518,#448,.T.);
#627=EDGE_CURVE('',#518,#519,#334,.T.);
#628=EDGE_CURVE('',#519,#519,#449,.T.);
#629=EDGE_CURVE('',#520,#520,#450,.T.);
#630=EDGE_CURVE('',#520,#521,#335,.T.);
#631=EDGE_CURVE('',#521,#521,#451,.T.);
#632=EDGE_CURVE('',#522,#523,#452,.T.);
#633=EDGE_CURVE('',#523,#524,#336,.T.);
#634=EDGE_CURVE('',#524,#524,#453,.T.);
#635=EDGE_CURVE('',#523,#525,#454,.T.);
#636=EDGE_CURVE('',#526,#525,#337,.T.);
#637=EDGE_CURVE('',#526,#527,#155,.T.);
#638=EDGE_CURVE('',#522,#527,#338,.T.);
#639=EDGE_CURVE('',#528,#522,#339,.T.);
#640=EDGE_CURVE('',#528,#529,#340,.T.);
#641=EDGE_CURVE('',#529,#525,#341,.T.);
#642=EDGE_CURVE('',#527,#530,#455,.T.);
#643=EDGE_CURVE('',#530,#528,#342,.T.);
#644=EDGE_CURVE('',#531,#529,#343,.T.);
#645=EDGE_CURVE('',#531,#526,#456,.T.);
#646=EDGE_CURVE('',#530,#531,#344,.T.);
#647=EDGE_CURVE('',#532,#533,#345,.T.);
#648=EDGE_CURVE('',#533,#534,#346,.T.);
#649=EDGE_CURVE('',#535,#534,#347,.T.);
#650=EDGE_CURVE('',#535,#532,#348,.T.);
#651=EDGE_CURVE('',#534,#536,#457,.T.);
#652=EDGE_CURVE('',#537,#536,#349,.T.);
#653=EDGE_CURVE('',#537,#535,#458,.T.);
#654=EDGE_CURVE('',#536,#538,#350,.T.);
#655=EDGE_CURVE('',#539,#538,#351,.T.);
#656=EDGE_CURVE('',#539,#537,#352,.T.);
#657=EDGE_CURVE('',#538,#533,#459,.T.);
#658=EDGE_CURVE('',#532,#539,#460,.T.);
#659=ORIENTED_EDGE('',*,*,#540,.T.);
#660=ORIENTED_EDGE('',*,*,#541,.T.);
#661=ORIENTED_EDGE('',*,*,#542,.F.);
#662=ORIENTED_EDGE('',*,*,#541,.F.);
#663=ORIENTED_EDGE('',*,*,#543,.T.);
#664=ORIENTED_EDGE('',*,*,#544,.T.);
#665=ORIENTED_EDGE('',*,*,#545,.F.);
#666=ORIENTED_EDGE('',*,*,#544,.F.);
#667=ORIENTED_EDGE('',*,*,#546,.T.);
#668=ORIENTED_EDGE('',*,*,#547,.T.);
#669=ORIENTED_EDGE('',*,*,#548,.T.);
#670=ORIENTED_EDGE('',*,*,#549,.F.);
#671=ORIENTED_EDGE('',*,*,#548,.F.);
#672=ORIENTED_EDGE('',*,*,#550,.T.);
#673=ORIENTED_EDGE('',*,*,#551,.T.);
#674=ORIENTED_EDGE('',*,*,#552,.F.);
#675=ORIENTED_EDGE('',*,*,#551,.F.);
#676=ORIENTED_EDGE('',*,*,#546,.F.);
#677=ORIENTED_EDGE('',*,*,#552,.T.);
#678=ORIENTED_EDGE('',*,*,#547,.F.);
#679=ORIENTED_EDGE('',*,*,#550,.F.);
#680=ORIENTED_EDGE('',*,*,#549,.T.);
#681=ORIENTED_EDGE('',*,*,#545,.T.);
#682=ORIENTED_EDGE('',*,*,#540,.F.);
#683=ORIENTED_EDGE('',*,*,#543,.F.);
#684=ORIENTED_EDGE('',*,*,#542,.T.);
#685=ORIENTED_EDGE('',*,*,#553,.F.);
#686=ORIENTED_EDGE('',*,*,#554,.T.);
#687=ORIENTED_EDGE('',*,*,#555,.F.);
#688=ORIENTED_EDGE('',*,*,#554,.F.);
#689=ORIENTED_EDGE('',*,*,#556,.F.);
#690=ORIENTED_EDGE('',*,*,#557,.T.);
#691=ORIENTED_EDGE('',*,*,#558,.T.);
#692=ORIENTED_EDGE('',*,*,#557,.F.);
#693=ORIENTED_EDGE('',*,*,#559,.F.);
#694=ORIENTED_EDGE('',*,*,#560,.F.);
#695=ORIENTED_EDGE('',*,*,#561,.T.);
#696=ORIENTED_EDGE('',*,*,#562,.F.);
#697=ORIENTED_EDGE('',*,*,#563,.F.);
#698=ORIENTED_EDGE('',*,*,#564,.T.);
#699=ORIENTED_EDGE('',*,*,#565,.T.);
#700=ORIENTED_EDGE('',*,*,#564,.F.);
#701=ORIENTED_EDGE('',*,*,#566,.F.);
#702=ORIENTED_EDGE('',*,*,#567,.T.);
#703=ORIENTED_EDGE('',*,*,#568,.T.);
#704=ORIENTED_EDGE('',*,*,#569,.T.);
#705=ORIENTED_EDGE('',*,*,#570,.F.);
#706=ORIENTED_EDGE('',*,*,#571,.T.);
#707=ORIENTED_EDGE('',*,*,#572,.T.);
#708=ORIENTED_EDGE('',*,*,#573,.T.);
#709=ORIENTED_EDGE('',*,*,#574,.T.);
#710=ORIENTED_EDGE('',*,*,#575,.T.);
#711=ORIENTED_EDGE('',*,*,#576,.F.);
#712=ORIENTED_EDGE('',*,*,#577,.F.);
#713=ORIENTED_EDGE('',*,*,#578,.F.);
#714=ORIENTED_EDGE('',*,*,#579,.F.);
#715=ORIENTED_EDGE('',*,*,#580,.F.);
#716=ORIENTED_EDGE('',*,*,#581,.F.);
#717=ORIENTED_EDGE('',*,*,#582,.F.);
#718=ORIENTED_EDGE('',*,*,#583,.T.);
#719=ORIENTED_EDGE('',*,*,#584,.F.);
#720=ORIENTED_EDGE('',*,*,#579,.T.);
#721=ORIENTED_EDGE('',*,*,#566,.T.);
#722=ORIENTED_EDGE('',*,*,#574,.F.);
#723=ORIENTED_EDGE('',*,*,#585,.T.);
#724=ORIENTED_EDGE('',*,*,#573,.F.);
#725=ORIENTED_EDGE('',*,*,#586,.F.);
#726=ORIENTED_EDGE('',*,*,#580,.T.);
#727=ORIENTED_EDGE('',*,*,#585,.F.);
#728=ORIENTED_EDGE('',*,*,#558,.F.);
#729=ORIENTED_EDGE('',*,*,#575,.F.);
#730=ORIENTED_EDGE('',*,*,#563,.T.);
#731=ORIENTED_EDGE('',*,*,#578,.T.);
#732=ORIENTED_EDGE('',*,*,#587,.F.);
#733=ORIENTED_EDGE('',*,*,#577,.T.);
#734=ORIENTED_EDGE('',*,*,#588,.T.);
#735=ORIENTED_EDGE('',*,*,#567,.F.);
#736=ORIENTED_EDGE('',*,*,#587,.T.);
#737=ORIENTED_EDGE('',*,*,#553,.T.);
#738=ORIENTED_EDGE('',*,*,#569,.F.);
#739=ORIENTED_EDGE('',*,*,#589,.T.);
#740=ORIENTED_EDGE('',*,*,#584,.T.);
#741=ORIENTED_EDGE('',*,*,#590,.F.);
#742=ORIENTED_EDGE('',*,*,#555,.T.);
#743=ORIENTED_EDGE('',*,*,#583,.F.);
#744=ORIENTED_EDGE('',*,*,#591,.F.);
#745=ORIENTED_EDGE('',*,*,#570,.T.);
#746=ORIENTED_EDGE('',*,*,#590,.T.);
#747=ORIENTED_EDGE('',*,*,#592,.F.);
#748=ORIENTED_EDGE('',*,*,#561,.F.);
#749=ORIENTED_EDGE('',*,*,#593,.F.);
#750=ORIENTED_EDGE('',*,*,#594,.F.);
#751=ORIENTED_EDGE('',*,*,#582,.T.);
#752=ORIENTED_EDGE('',*,*,#595,.T.);
#753=ORIENTED_EDGE('',*,*,#571,.F.);
#754=ORIENTED_EDGE('',*,*,#591,.T.);
#755=ORIENTED_EDGE('',*,*,#556,.T.);
#756=ORIENTED_EDGE('',*,*,#565,.F.);
#757=ORIENTED_EDGE('',*,*,#596,.F.);
#758=ORIENTED_EDGE('',*,*,#597,.F.);
#759=ORIENTED_EDGE('',*,*,#598,.F.);
#760=ORIENTED_EDGE('',*,*,#559,.T.);
#761=ORIENTED_EDGE('',*,*,#586,.T.);
#762=ORIENTED_EDGE('',*,*,#572,.F.);
#763=ORIENTED_EDGE('',*,*,#595,.F.);
#764=ORIENTED_EDGE('',*,*,#581,.T.);
#765=ORIENTED_EDGE('',*,*,#576,.T.);
#766=ORIENTED_EDGE('',*,*,#589,.F.);
#767=ORIENTED_EDGE('',*,*,#568,.F.);
#768=ORIENTED_EDGE('',*,*,#588,.F.);
#769=ORIENTED_EDGE('',*,*,#592,.T.);
#770=ORIENTED_EDGE('',*,*,#599,.T.);
#771=ORIENTED_EDGE('',*,*,#596,.T.);
#772=ORIENTED_EDGE('',*,*,#562,.T.);
#773=ORIENTED_EDGE('',*,*,#594,.T.);
#774=ORIENTED_EDGE('',*,*,#600,.T.);
#775=ORIENTED_EDGE('',*,*,#597,.T.);
#776=ORIENTED_EDGE('',*,*,#599,.F.);
#777=ORIENTED_EDGE('',*,*,#593,.T.);
#778=ORIENTED_EDGE('',*,*,#560,.T.);
#779=ORIENTED_EDGE('',*,*,#598,.T.);
#780=ORIENTED_EDGE('',*,*,#600,.F.);
#781=ORIENTED_EDGE('',*,*,#601,.F.);
#782=ORIENTED_EDGE('',*,*,#602,.T.);
#783=ORIENTED_EDGE('',*,*,#603,.F.);
#784=ORIENTED_EDGE('',*,*,#604,.F.);
#785=ORIENTED_EDGE('',*,*,#602,.F.);
#786=ORIENTED_EDGE('',*,*,#605,.F.);
#787=ORIENTED_EDGE('',*,*,#606,.T.);
#788=ORIENTED_EDGE('',*,*,#607,.F.);
#789=ORIENTED_EDGE('',*,*,#606,.F.);
#790=ORIENTED_EDGE('',*,*,#608,.F.);
#791=ORIENTED_EDGE('',*,*,#609,.T.);
#792=ORIENTED_EDGE('',*,*,#610,.T.);
#793=ORIENTED_EDGE('',*,*,#603,.T.);
#794=ORIENTED_EDGE('',*,*,#604,.T.);
#795=ORIENTED_EDGE('',*,*,#610,.F.);
#796=ORIENTED_EDGE('',*,*,#611,.F.);
#797=ORIENTED_EDGE('',*,*,#612,.T.);
#798=ORIENTED_EDGE('',*,*,#605,.T.);
#799=ORIENTED_EDGE('',*,*,#613,.T.);
#800=ORIENTED_EDGE('',*,*,#614,.T.);
#801=ORIENTED_EDGE('',*,*,#613,.F.);
#802=ORIENTED_EDGE('',*,*,#608,.T.);
#803=ORIENTED_EDGE('',*,*,#612,.F.);
#804=ORIENTED_EDGE('',*,*,#607,.T.);
#805=ORIENTED_EDGE('',*,*,#601,.T.);
#806=ORIENTED_EDGE('',*,*,#609,.F.);
#807=ORIENTED_EDGE('',*,*,#611,.T.);
#808=ORIENTED_EDGE('',*,*,#614,.F.);
#809=ORIENTED_EDGE('',*,*,#615,.F.);
#810=ORIENTED_EDGE('',*,*,#616,.T.);
#811=ORIENTED_EDGE('',*,*,#617,.T.);
#812=ORIENTED_EDGE('',*,*,#618,.T.);
#813=ORIENTED_EDGE('',*,*,#616,.F.);
#814=ORIENTED_EDGE('',*,*,#619,.T.);
#815=ORIENTED_EDGE('',*,*,#620,.T.);
#816=ORIENTED_EDGE('',*,*,#621,.F.);
#817=ORIENTED_EDGE('',*,*,#620,.F.);
#818=ORIENTED_EDGE('',*,*,#622,.T.);
#819=ORIENTED_EDGE('',*,*,#623,.T.);
#820=ORIENTED_EDGE('',*,*,#624,.T.);
#821=ORIENTED_EDGE('',*,*,#625,.F.);
#822=ORIENTED_EDGE('',*,*,#624,.F.);
#823=ORIENTED_EDGE('',*,*,#619,.F.);
#824=ORIENTED_EDGE('',*,*,#622,.F.);
#825=ORIENTED_EDGE('',*,*,#618,.F.);
#826=ORIENTED_EDGE('',*,*,#617,.F.);
#827=ORIENTED_EDGE('',*,*,#626,.T.);
#828=ORIENTED_EDGE('',*,*,#627,.T.);
#829=ORIENTED_EDGE('',*,*,#628,.F.);
#830=ORIENTED_EDGE('',*,*,#627,.F.);
#831=ORIENTED_EDGE('',*,*,#615,.T.);
#832=ORIENTED_EDGE('',*,*,#621,.T.);
#833=ORIENTED_EDGE('',*,*,#628,.T.);
#834=ORIENTED_EDGE('',*,*,#623,.F.);
#835=ORIENTED_EDGE('',*,*,#626,.F.);
#836=ORIENTED_EDGE('',*,*,#625,.T.);
#837=ORIENTED_EDGE('',*,*,#629,.T.);
#838=ORIENTED_EDGE('',*,*,#630,.T.);
#839=ORIENTED_EDGE('',*,*,#631,.F.);
#840=ORIENTED_EDGE('',*,*,#630,.F.);
#841=ORIENTED_EDGE('',*,*,#631,.T.);
#842=ORIENTED_EDGE('',*,*,#629,.F.);
#843=ORIENTED_EDGE('',*,*,#632,.T.);
#844=ORIENTED_EDGE('',*,*,#633,.T.);
#845=ORIENTED_EDGE('',*,*,#634,.F.);
#846=ORIENTED_EDGE('',*,*,#633,.F.);
#847=ORIENTED_EDGE('',*,*,#635,.T.);
#848=ORIENTED_EDGE('',*,*,#636,.F.);
#849=ORIENTED_EDGE('',*,*,#637,.T.);
#850=ORIENTED_EDGE('',*,*,#638,.F.);
#851=ORIENTED_EDGE('',*,*,#639,.F.);
#852=ORIENTED_EDGE('',*,*,#640,.T.);
#853=ORIENTED_EDGE('',*,*,#641,.T.);
#854=ORIENTED_EDGE('',*,*,#635,.F.);
#855=ORIENTED_EDGE('',*,*,#632,.F.);
#856=ORIENTED_EDGE('',*,*,#634,.T.);
#857=ORIENTED_EDGE('',*,*,#638,.T.);
#858=ORIENTED_EDGE('',*,*,#642,.T.);
#859=ORIENTED_EDGE('',*,*,#643,.T.);
#860=ORIENTED_EDGE('',*,*,#639,.T.);
#861=ORIENTED_EDGE('',*,*,#644,.F.);
#862=ORIENTED_EDGE('',*,*,#645,.T.);
#863=ORIENTED_EDGE('',*,*,#636,.T.);
#864=ORIENTED_EDGE('',*,*,#641,.F.);
#865=ORIENTED_EDGE('',*,*,#643,.F.);
#866=ORIENTED_EDGE('',*,*,#646,.T.);
#867=ORIENTED_EDGE('',*,*,#644,.T.);
#868=ORIENTED_EDGE('',*,*,#640,.F.);
#869=ORIENTED_EDGE('',*,*,#642,.F.);
#870=ORIENTED_EDGE('',*,*,#637,.F.);
#871=ORIENTED_EDGE('',*,*,#645,.F.);
#872=ORIENTED_EDGE('',*,*,#646,.F.);
#873=ORIENTED_EDGE('',*,*,#647,.T.);
#874=ORIENTED_EDGE('',*,*,#648,.T.);
#875=ORIENTED_EDGE('',*,*,#649,.F.);
#876=ORIENTED_EDGE('',*,*,#650,.T.);
#877=ORIENTED_EDGE('',*,*,#651,.T.);
#878=ORIENTED_EDGE('',*,*,#652,.F.);
#879=ORIENTED_EDGE('',*,*,#653,.T.);
#880=ORIENTED_EDGE('',*,*,#649,.T.);
#881=ORIENTED_EDGE('',*,*,#652,.T.);
#882=ORIENTED_EDGE('',*,*,#654,.T.);
#883=ORIENTED_EDGE('',*,*,#655,.F.);
#884=ORIENTED_EDGE('',*,*,#656,.T.);
#885=ORIENTED_EDGE('',*,*,#655,.T.);
#886=ORIENTED_EDGE('',*,*,#657,.T.);
#887=ORIENTED_EDGE('',*,*,#647,.F.);
#888=ORIENTED_EDGE('',*,*,#658,.T.);
#889=ORIENTED_EDGE('',*,*,#651,.F.);
#890=ORIENTED_EDGE('',*,*,#648,.F.);
#891=ORIENTED_EDGE('',*,*,#657,.F.);
#892=ORIENTED_EDGE('',*,*,#654,.F.);
#893=ORIENTED_EDGE('',*,*,#650,.F.);
#894=ORIENTED_EDGE('',*,*,#653,.F.);
#895=ORIENTED_EDGE('',*,*,#656,.F.);
#896=ORIENTED_EDGE('',*,*,#658,.F.);
#897=CYLINDRICAL_SURFACE('',#1062,15.);
#898=CYLINDRICAL_SURFACE('',#1065,25.);
#899=CYLINDRICAL_SURFACE('',#1068,15.);
#900=CYLINDRICAL_SURFACE('',#1071,25.);
#901=CYLINDRICAL_SURFACE('',#1079,15.0000000000001);
#902=CYLINDRICAL_SURFACE('',#1082,15.0000000000001);
#903=CYLINDRICAL_SURFACE('',#1085,25.0000000000002);
#904=CYLINDRICAL_SURFACE('',#1088,45.0000000000003);
#905=CYLINDRICAL_SURFACE('',#1106,45.0000000000003);
#906=CYLINDRICAL_SURFACE('',#1107,45.0000000000003);
#907=CYLINDRICAL_SURFACE('',#1117,2.5);
#908=CYLINDRICAL_SURFACE('',#1118,25.);
#909=CYLINDRICAL_SURFACE('',#1120,15.);
#910=CYLINDRICAL_SURFACE('',#1127,2.49999999999999);
#911=CYLINDRICAL_SURFACE('',#1128,2.49999999999999);
#912=CYLINDRICAL_SURFACE('',#1129,15.);
#913=CYLINDRICAL_SURFACE('',#1132,25.);
#914=CYLINDRICAL_SURFACE('',#1138,2.49999999999999);
#915=CYLINDRICAL_SURFACE('',#1144,25.0000000000002);
#916=CYLINDRICAL_SURFACE('',#1155,10.0000000000001);
#917=CYLINDRICAL_SURFACE('',#1165,10.0000000000001);
#918=CYLINDRICAL_SURFACE('',#1166,10.0000000000001);
#919=ADVANCED_FACE('',(#156),#897,.F.);
#920=ADVANCED_FACE('',(#157,#125),#898,.T.);
#921=ADVANCED_FACE('',(#158),#899,.F.);
#922=ADVANCED_FACE('',(#159,#126),#900,.T.);
#923=ADVANCED_FACE('',(#160,#127),#92,.T.);
#924=ADVANCED_FACE('',(#161,#128),#93,.F.);
#925=ADVANCED_FACE('',(#162,#129),#94,.T.);
#926=ADVANCED_FACE('',(#163,#130),#95,.F.);
#927=ADVANCED_FACE('',(#164),#901,.F.);
#928=ADVANCED_FACE('',(#165),#902,.F.);
#929=ADVANCED_FACE('',(#166),#903,.F.);
#930=ADVANCED_FACE('',(#167),#904,.T.);
#931=ADVANCED_FACE('',(#168),#96,.T.);
#932=ADVANCED_FACE('',(#169),#97,.F.);
#933=ADVANCED_FACE('',(#170),#98,.F.);
#934=ADVANCED_FACE('',(#171,#131),#99,.F.);
#935=ADVANCED_FACE('',(#172),#100,.F.);
#936=ADVANCED_FACE('',(#173,#132),#101,.F.);
#937=ADVANCED_FACE('',(#174,#133),#102,.F.);
#938=ADVANCED_FACE('',(#175,#134),#103,.T.);
#939=ADVANCED_FACE('',(#176,#135),#104,.F.);
#940=ADVANCED_FACE('',(#177,#136),#105,.T.);
#941=ADVANCED_FACE('',(#178),#905,.T.);
#942=ADVANCED_FACE('',(#179),#906,.T.);
#943=ADVANCED_FACE('',(#180),#106,.F.);
#944=ADVANCED_FACE('',(#181),#107,.F.);
#945=ADVANCED_FACE('',(#182),#108,.F.);
#946=ADVANCED_FACE('',(#183),#63,.T.);
#947=ADVANCED_FACE('',(#184),#907,.F.);
#948=ADVANCED_FACE('',(#185),#908,.T.);
#949=ADVANCED_FACE('',(#186,#137),#909,.T.);
#950=ADVANCED_FACE('',(#187),#109,.T.);
#951=ADVANCED_FACE('',(#188,#138),#110,.F.);
#952=ADVANCED_FACE('',(#189),#111,.F.);
#953=ADVANCED_FACE('',(#190),#910,.F.);
#954=ADVANCED_FACE('',(#191),#911,.F.);
#955=ADVANCED_FACE('',(#192,#139,#140),#912,.F.);
#956=ADVANCED_FACE('',(#193,#141,#142),#913,.T.);
#957=ADVANCED_FACE('',(#194,#143),#112,.T.);
#958=ADVANCED_FACE('',(#195,#144),#113,.F.);
#959=ADVANCED_FACE('',(#196),#914,.T.);
#960=ADVANCED_FACE('',(#197),#114,.T.);
#961=ADVANCED_FACE('',(#198),#115,.F.);
#962=ADVANCED_FACE('',(#199),#915,.T.);
#963=ADVANCED_FACE('',(#200),#116,.F.);
#964=ADVANCED_FACE('',(#201),#117,.T.);
#965=ADVANCED_FACE('',(#202),#118,.T.);
#966=ADVANCED_FACE('',(#203),#119,.T.);
#967=ADVANCED_FACE('',(#204),#120,.T.);
#968=ADVANCED_FACE('',(#205),#916,.F.);
#969=ADVANCED_FACE('',(#206),#121,.F.);
#970=ADVANCED_FACE('',(#207),#122,.F.);
#971=ADVANCED_FACE('',(#208),#123,.F.);
#972=ADVANCED_FACE('',(#209),#124,.F.);
#973=ADVANCED_FACE('',(#210),#917,.T.);
#974=ADVANCED_FACE('',(#211),#918,.T.);
#975=CLOSED_SHELL('',(#919,#920,#921,#922,#923,#924,#925,#926));
#976=CLOSED_SHELL('',(#927,#928,#929,#930,#931,#932,#933,#934,#935,#936,
#937,#938,#939,#940,#941,#942,#943,#944,#945));
#977=CLOSED_SHELL('',(#946,#947,#948,#949,#950,#951,#952));
#978=CLOSED_SHELL('',(#953,#954,#955,#956,#957,#958));
#979=CLOSED_SHELL('',(#959,#960,#961));
#980=CLOSED_SHELL('',(#962,#963,#964,#965,#966,#967,#968));
#981=CLOSED_SHELL('',(#969,#970,#971,#972,#973,#974));
#982=DERIVED_UNIT_ELEMENT(#996,1.);
#983=DERIVED_UNIT_ELEMENT(#2061,-3.);
#984=DERIVED_UNIT_ELEMENT(#996,1.);
#985=DERIVED_UNIT_ELEMENT(#2061,-3.);
#986=DERIVED_UNIT_ELEMENT(#996,1.);
#987=DERIVED_UNIT_ELEMENT(#2061,-3.);
#988=DERIVED_UNIT_ELEMENT(#996,1.);
#989=DERIVED_UNIT_ELEMENT(#2061,-3.);
#990=DERIVED_UNIT_ELEMENT(#996,1.);
#991=DERIVED_UNIT_ELEMENT(#2061,-3.);
#992=DERIVED_UNIT_ELEMENT(#996,1.);
#993=DERIVED_UNIT_ELEMENT(#2061,-3.);
#994=DERIVED_UNIT_ELEMENT(#996,1.);
#995=DERIVED_UNIT_ELEMENT(#2061,-3.);
#996=(
MASS_UNIT()
NAMED_UNIT(*)
SI_UNIT(.KILO.,.GRAM.)
);
#997=DERIVED_UNIT((#982,#983));
#998=DERIVED_UNIT((#984,#985));
#999=DERIVED_UNIT((#986,#987));
#1000=DERIVED_UNIT((#988,#989));
#1001=DERIVED_UNIT((#990,#991));
#1002=DERIVED_UNIT((#992,#993));
#1003=DERIVED_UNIT((#994,#995));
#1004=MEASURE_REPRESENTATION_ITEM('density measure',
POSITIVE_RATIO_MEASURE(7850.),#997);
#1005=MEASURE_REPRESENTATION_ITEM('density measure',
POSITIVE_RATIO_MEASURE(7850.),#998);
#1006=MEASURE_REPRESENTATION_ITEM('density measure',
POSITIVE_RATIO_MEASURE(7850.),#999);
#1007=MEASURE_REPRESENTATION_ITEM('density measure',
POSITIVE_RATIO_MEASURE(7850.),#1000);
#1008=MEASURE_REPRESENTATION_ITEM('density measure',
POSITIVE_RATIO_MEASURE(7850.),#1001);
#1009=MEASURE_REPRESENTATION_ITEM('density measure',
POSITIVE_RATIO_MEASURE(7850.),#1002);
#1010=MEASURE_REPRESENTATION_ITEM('density measure',
POSITIVE_RATIO_MEASURE(7850.),#1003);
#1011=PROPERTY_DEFINITION_REPRESENTATION(#1046,#1025);
#1012=PROPERTY_DEFINITION_REPRESENTATION(#1047,#1026);
#1013=PROPERTY_DEFINITION_REPRESENTATION(#1048,#1027);
#1014=PROPERTY_DEFINITION_REPRESENTATION(#1049,#1028);
#1015=PROPERTY_DEFINITION_REPRESENTATION(#1050,#1029);
#1016=PROPERTY_DEFINITION_REPRESENTATION(#1051,#1030);
#1017=PROPERTY_DEFINITION_REPRESENTATION(#1052,#1031);
#1018=PROPERTY_DEFINITION_REPRESENTATION(#1053,#1032);
#1019=PROPERTY_DEFINITION_REPRESENTATION(#1054,#1033);
#1020=PROPERTY_DEFINITION_REPRESENTATION(#1055,#1034);
#1021=PROPERTY_DEFINITION_REPRESENTATION(#1056,#1035);
#1022=PROPERTY_DEFINITION_REPRESENTATION(#1057,#1036);
#1023=PROPERTY_DEFINITION_REPRESENTATION(#1058,#1037);
#1024=PROPERTY_DEFINITION_REPRESENTATION(#1059,#1038);
#1025=REPRESENTATION('material name',(#1039),#2052);
#1026=REPRESENTATION('density',(#1004),#2052);
#1027=REPRESENTATION('material name',(#1040),#2053);
#1028=REPRESENTATION('density',(#1005),#2053);
#1029=REPRESENTATION('material name',(#1041),#2054);
#1030=REPRESENTATION('density',(#1006),#2054);
#1031=REPRESENTATION('material name',(#1042),#2055);
#1032=REPRESENTATION('density',(#1007),#2055);
#1033=REPRESENTATION('material name',(#1043),#2056);
#1034=REPRESENTATION('density',(#1008),#2056);
#1035=REPRESENTATION('material name',(#1044),#2057);
#1036=REPRESENTATION('density',(#1009),#2057);
#1037=REPRESENTATION('material name',(#1045),#2058);
#1038=REPRESENTATION('density',(#1010),#2058);
#1039=DESCRIPTIVE_REPRESENTATION_ITEM('Steel','Steel');
#1040=DESCRIPTIVE_REPRESENTATION_ITEM('Steel','Steel');
#1041=DESCRIPTIVE_REPRESENTATION_ITEM('Steel','Steel');
#1042=DESCRIPTIVE_REPRESENTATION_ITEM('Steel','Steel');
#1043=DESCRIPTIVE_REPRESENTATION_ITEM('Steel','Steel');
#1044=DESCRIPTIVE_REPRESENTATION_ITEM('Steel','Steel');
#1045=DESCRIPTIVE_REPRESENTATION_ITEM('Steel','Steel');
#1046=PROPERTY_DEFINITION('material property','material name',#2103);
#1047=PROPERTY_DEFINITION('material property','density of part',#2103);
#1048=PROPERTY_DEFINITION('material property','material name',#2104);
#1049=PROPERTY_DEFINITION('material property','density of part',#2104);
#1050=PROPERTY_DEFINITION('material property','material name',#2105);
#1051=PROPERTY_DEFINITION('material property','density of part',#2105);
#1052=PROPERTY_DEFINITION('material property','material name',#2106);
#1053=PROPERTY_DEFINITION('material property','density of part',#2106);
#1054=PROPERTY_DEFINITION('material property','material name',#2107);
#1055=PROPERTY_DEFINITION('material property','density of part',#2107);
#1056=PROPERTY_DEFINITION('material property','material name',#2108);
#1057=PROPERTY_DEFINITION('material property','density of part',#2108);
#1058=PROPERTY_DEFINITION('material property','material name',#2109);
#1059=PROPERTY_DEFINITION('material property','density of part',#2109);
#1060=AXIS2_PLACEMENT_3D('',#1485,#1180,#1181);
#1061=AXIS2_PLACEMENT_3D('',#1486,#1182,#1183);
#1062=AXIS2_PLACEMENT_3D('',#1487,#1184,#1185);
#1063=AXIS2_PLACEMENT_3D('',#1489,#1186,#1187);
#1064=AXIS2_PLACEMENT_3D('',#1492,#1189,#1190);
#1065=AXIS2_PLACEMENT_3D('',#1493,#1191,#1192);
#1066=AXIS2_PLACEMENT_3D('',#1495,#1193,#1194);
#1067=AXIS2_PLACEMENT_3D('',#1498,#1196,#1197);
#1068=AXIS2_PLACEMENT_3D('',#1566,#1198,#1199);
#1069=AXIS2_PLACEMENT_3D('',#1568,#1200,#1201);
#1070=AXIS2_PLACEMENT_3D('',#1571,#1203,#1204);
#1071=AXIS2_PLACEMENT_3D('',#1572,#1205,#1206);
#1072=AXIS2_PLACEMENT_3D('',#1574,#1207,#1208);
#1073=AXIS2_PLACEMENT_3D('',#1577,#1210,#1211);
#1074=AXIS2_PLACEMENT_3D('',#1578,#1212,#1213);
#1075=AXIS2_PLACEMENT_3D('',#1579,#1214,#1215);
#1076=AXIS2_PLACEMENT_3D('',#1580,#1216,#1217);
#1077=AXIS2_PLACEMENT_3D('',#1581,#1218,#1219);
#1078=AXIS2_PLACEMENT_3D('',#1582,#1220,#1221);
#1079=AXIS2_PLACEMENT_3D('',#1583,#1222,#1223);
#1080=AXIS2_PLACEMENT_3D('',#1585,#1224,#1225);
#1081=AXIS2_PLACEMENT_3D('',#1588,#1227,#1228);
#1082=AXIS2_PLACEMENT_3D('',#1589,#1229,#1230);
#1083=AXIS2_PLACEMENT_3D('',#1591,#1231,#1232);
#1084=AXIS2_PLACEMENT_3D('',#1594,#1234,#1235);
#1085=AXIS2_PLACEMENT_3D('',#1595,#1236,#1237);
#1086=AXIS2_PLACEMENT_3D('',#1598,#1238,#1239);
#1087=AXIS2_PLACEMENT_3D('',#1602,#1241,#1242);
#1088=AXIS2_PLACEMENT_3D('',#1604,#1244,#1245);
#1089=AXIS2_PLACEMENT_3D('',#1607,#1246,#1247);
#1090=AXIS2_PLACEMENT_3D('',#1610,#1249,#1250);
#1091=AXIS2_PLACEMENT_3D('',#1611,#1251,#1252);
#1092=AXIS2_PLACEMENT_3D('',#1612,#1253,#1254);
#1093=AXIS2_PLACEMENT_3D('',#1630,#1264,#1265);
#1094=AXIS2_PLACEMENT_3D('',#1648,#1275,#1276);
#1095=AXIS2_PLACEMENT_3D('',#1650,#1278,#1279);
#1096=AXIS2_PLACEMENT_3D('',#1651,#1280,#1281);
#1097=AXIS2_PLACEMENT_3D('',#1652,#1282,#1283);
#1098=AXIS2_PLACEMENT_3D('',#1654,#1285,#1286);
#1099=AXIS2_PLACEMENT_3D('',#1655,#1287,#1288);
#1100=AXIS2_PLACEMENT_3D('',#1656,#1289,#1290);
#1101=AXIS2_PLACEMENT_3D('',#1657,#1291,#1292);
#1102=AXIS2_PLACEMENT_3D('',#1659,#1294,#1295);
#1103=AXIS2_PLACEMENT_3D('',#1666,#1300,#1301);
#1104=AXIS2_PLACEMENT_3D('',#1667,#1302,#1303);
#1105=AXIS2_PLACEMENT_3D('',#1668,#1304,#1305);
#1106=AXIS2_PLACEMENT_3D('',#1674,#1309,#1310);
#1107=AXIS2_PLACEMENT_3D('',#1675,#1311,#1312);
#1108=AXIS2_PLACEMENT_3D('',#1676,#1313,#1314);
#1109=AXIS2_PLACEMENT_3D('',#1678,#1316,#1317);
#1110=AXIS2_PLACEMENT_3D('',#1680,#1319,#1320);
#1111=AXIS2_PLACEMENT_3D('',#1681,#1321,#1322);
#1112=AXIS2_PLACEMENT_3D('',#1682,#1323,#1324);
#1113=AXIS2_PLACEMENT_3D('',#1684,#1325,#1326);
#1114=AXIS2_PLACEMENT_3D('',#1686,#1327,#1328);
#1115=AXIS2_PLACEMENT_3D('',#1688,#1329,#1330);
#1116=AXIS2_PLACEMENT_3D('',#1689,#1331,#1332);
#1117=AXIS2_PLACEMENT_3D('',#1690,#1333,#1334);
#1118=AXIS2_PLACEMENT_3D('',#1766,#1336,#1337);
#1119=AXIS2_PLACEMENT_3D('',#1768,#1338,#1339);
#1120=AXIS2_PLACEMENT_3D('',#1770,#1341,#1342);
#1121=AXIS2_PLACEMENT_3D('',#1772,#1343,#1344);
#1122=AXIS2_PLACEMENT_3D('',#1776,#1347,#1348);
#1123=AXIS2_PLACEMENT_3D('',#1777,#1349,#1350);
#1124=AXIS2_PLACEMENT_3D('',#1778,#1351,#1352);
#1125=AXIS2_PLACEMENT_3D('',#1779,#1353,#1354);
#1126=AXIS2_PLACEMENT_3D('',#1780,#1355,#1356);
#1127=AXIS2_PLACEMENT_3D('',#1781,#1357,#1358);
#1128=AXIS2_PLACEMENT_3D('',#1857,#1360,#1361);
#1129=AXIS2_PLACEMENT_3D('',#1933,#1363,#1364);
#1130=AXIS2_PLACEMENT_3D('',#1935,#1365,#1366);
#1131=AXIS2_PLACEMENT_3D('',#1938,#1368,#1369);
#1132=AXIS2_PLACEMENT_3D('',#1939,#1370,#1371);
#1133=AXIS2_PLACEMENT_3D('',#1941,#1372,#1373);
#1134=AXIS2_PLACEMENT_3D('',#1944,#1375,#1376);
#1135=AXIS2_PLACEMENT_3D('',#1945,#1377,#1378);
#1136=AXIS2_PLACEMENT_3D('',#1946,#1379,#1380);
#1137=AXIS2_PLACEMENT_3D('',#1947,#1381,#1382);
#1138=AXIS2_PLACEMENT_3D('',#1948,#1383,#1384);
#1139=AXIS2_PLACEMENT_3D('',#1950,#1385,#1386);
#1140=AXIS2_PLACEMENT_3D('',#1953,#1388,#1389);
#1141=AXIS2_PLACEMENT_3D('',#1954,#1390,#1391);
#1142=AXIS2_PLACEMENT_3D('',#1955,#1392,#1393);
#1143=AXIS2_PLACEMENT_3D('',#1956,#1394,#1395);
#1144=AXIS2_PLACEMENT_3D('',#1957,#1396,#1397);
#1145=AXIS2_PLACEMENT_3D('',#1960,#1398,#1399);
#1146=AXIS2_PLACEMENT_3D('',#1963,#1401,#1402);
#1147=AXIS2_PLACEMENT_3D('',#1965,#1403,#1404);
#1148=AXIS2_PLACEMENT_3D('',#1984,#1407,#1408);
#1149=AXIS2_PLACEMENT_3D('',#1990,#1412,#1413);
#1150=AXIS2_PLACEMENT_3D('',#1991,#1414,#1415);
#1151=AXIS2_PLACEMENT_3D('',#1993,#1416,#1417);
#1152=AXIS2_PLACEMENT_3D('',#1995,#1419,#1420);
#1153=AXIS2_PLACEMENT_3D('',#1998,#1422,#1423);
#1154=AXIS2_PLACEMENT_3D('',#1999,#1424,#1425);
#1155=AXIS2_PLACEMENT_3D('',#2001,#1427,#1428);
#1156=AXIS2_PLACEMENT_3D('',#2002,#1429,#1430);
#1157=AXIS2_PLACEMENT_3D('',#2003,#1431,#1432);
#1158=AXIS2_PLACEMENT_3D('',#2012,#1437,#1438);
#1159=AXIS2_PLACEMENT_3D('',#2014,#1439,#1440);
#1160=AXIS2_PLACEMENT_3D('',#2017,#1442,#1443);
#1161=AXIS2_PLACEMENT_3D('',#2018,#1444,#1445);
#1162=AXIS2_PLACEMENT_3D('',#2024,#1449,#1450);
#1163=AXIS2_PLACEMENT_3D('',#2025,#1451,#1452);
#1164=AXIS2_PLACEMENT_3D('',#2026,#1453,#1454);
#1165=AXIS2_PLACEMENT_3D('',#2027,#1455,#1456);
#1166=AXIS2_PLACEMENT_3D('',#2028,#1457,#1458);
#1167=AXIS2_PLACEMENT_3D('',#2029,#1459,#1460);
#1168=AXIS2_PLACEMENT_3D('',#2030,#1461,#1462);
#1169=AXIS2_PLACEMENT_3D('',#2031,#1463,#1464);
#1170=AXIS2_PLACEMENT_3D('',#2032,#1465,#1466);
#1171=AXIS2_PLACEMENT_3D('',#2033,#1467,#1468);
#1172=AXIS2_PLACEMENT_3D('',#2034,#1469,#1470);
#1173=AXIS2_PLACEMENT_3D('',#2035,#1471,#1472);
#1174=AXIS2_PLACEMENT_3D('',#2036,#1473,#1474);
#1175=AXIS2_PLACEMENT_3D('',#2037,#1475,#1476);
#1176=AXIS2_PLACEMENT_3D('',#2038,#1477,#1478);
#1177=AXIS2_PLACEMENT_3D('',#2039,#1479,#1480);
#1178=AXIS2_PLACEMENT_3D('',#2040,#1481,#1482);
#1179=AXIS2_PLACEMENT_3D('',#2041,#1483,#1484);
#1180=DIRECTION('axis',(0.,0.,1.));
#1181=DIRECTION('refdir',(1.,0.,0.));
#1182=DIRECTION('axis',(0.,0.,1.));
#1183=DIRECTION('refdir',(1.,0.,0.));
#1184=DIRECTION('center_axis',(0.,-1.,0.));
#1185=DIRECTION('ref_axis',(0.,0.,-1.));
#1186=DIRECTION('center_axis',(0.,1.,0.));
#1187=DIRECTION('ref_axis',(0.,0.,1.));
#1188=DIRECTION('',(0.,-1.,0.));
#1189=DIRECTION('center_axis',(0.,1.,0.));
#1190=DIRECTION('ref_axis',(0.,0.,1.));
#1191=DIRECTION('center_axis',(0.,-1.,0.));
#1192=DIRECTION('ref_axis',(0.,0.,-1.));
#1193=DIRECTION('center_axis',(0.,1.,0.));
#1194=DIRECTION('ref_axis',(0.,0.,1.));
#1195=DIRECTION('',(0.,1.,0.));
#1196=DIRECTION('center_axis',(0.,1.,0.));
#1197=DIRECTION('ref_axis',(0.,0.,1.));
#1198=DIRECTION('center_axis',(0.,0.,-1.));
#1199=DIRECTION('ref_axis',(-1.,0.,0.));
#1200=DIRECTION('center_axis',(0.,0.,1.));
#1201=DIRECTION('ref_axis',(1.,0.,0.));
#1202=DIRECTION('',(0.,0.,-1.));
#1203=DIRECTION('center_axis',(0.,0.,1.));
#1204=DIRECTION('ref_axis',(1.,0.,0.));
#1205=DIRECTION('center_axis',(0.,0.,-1.));
#1206=DIRECTION('ref_axis',(-1.,0.,0.));
#1207=DIRECTION('center_axis',(0.,0.,1.));
#1208=DIRECTION('ref_axis',(1.,0.,0.));
#1209=DIRECTION('',(0.,0.,1.));
#1210=DIRECTION('center_axis',(0.,0.,1.));
#1211=DIRECTION('ref_axis',(1.,0.,0.));
#1212=DIRECTION('center_axis',(0.,0.,1.));
#1213=DIRECTION('ref_axis',(1.,0.,0.));
#1214=DIRECTION('center_axis',(0.,0.,1.));
#1215=DIRECTION('ref_axis',(1.,0.,0.));
#1216=DIRECTION('center_axis',(0.,1.,0.));
#1217=DIRECTION('ref_axis',(0.,0.,1.));
#1218=DIRECTION('center_axis',(0.,1.,0.));
#1219=DIRECTION('ref_axis',(0.,0.,1.));
#1220=DIRECTION('axis',(0.,0.,1.));
#1221=DIRECTION('refdir',(1.,0.,0.));
#1222=DIRECTION('center_axis',(-8.09275762631517E-30,1.,-3.72243739651165E-30));
#1223=DIRECTION('ref_axis',(-3.01247836291004E-59,3.72243739651165E-30,
1.));
#1224=DIRECTION('center_axis',(-8.09237244032629E-30,1.,-3.72243739651165E-30));
#1225=DIRECTION('ref_axis',(-3.01233497983708E-59,3.72243739651165E-30,
1.));
#1226=DIRECTION('',(-8.09275762631517E-30,1.,-3.72243739651165E-30));
#1227=DIRECTION('center_axis',(8.09237244032629E-30,-1.,3.72243739651165E-30));
#1228=DIRECTION('ref_axis',(3.01233497983708E-59,-3.72243739651165E-30,
-1.));
#1229=DIRECTION('center_axis',(-8.09275762631517E-30,1.,-3.72243739651165E-30));
#1230=DIRECTION('ref_axis',(-3.01247836291004E-59,3.72243739651165E-30,
1.));
#1231=DIRECTION('center_axis',(-8.09237244032629E-30,1.,-3.72243739651165E-30));
#1232=DIRECTION('ref_axis',(-3.01233497983708E-59,3.72243739651165E-30,
1.));
#1233=DIRECTION('',(-8.09275762631517E-30,1.,-3.72243739651165E-30));
#1234=DIRECTION('center_axis',(-8.09275762631517E-30,1.,-3.72243739651165E-30));
#1235=DIRECTION('ref_axis',(-3.01247836291004E-59,3.72243739651165E-30,
1.));
#1236=DIRECTION('center_axis',(1.,-7.90786835165394E-30,1.38777878078144E-17));
#1237=DIRECTION('ref_axis',(-7.96009957174572E-30,-1.,3.7364106986726E-15));
#1238=DIRECTION('center_axis',(1.,-7.90786835165394E-30,1.38777878078144E-17));
#1239=DIRECTION('ref_axis',(1.38777878078144E-17,-1.09743718996384E-46,
-1.));
#1240=DIRECTION('',(-1.,7.90786835165394E-30,-1.38777878078144E-17));
#1241=DIRECTION('center_axis',(1.,-8.05423902742737E-30,1.04083408558608E-17));
#1242=DIRECTION('ref_axis',(1.04083408558608E-17,-8.38312651320406E-47,
-1.));
#1243=DIRECTION('',(1.,-7.90786835165394E-30,1.38777878078144E-17));
#1244=DIRECTION('center_axis',(1.,-7.90786835165394E-30,1.38777878078144E-17));
#1245=DIRECTION('ref_axis',(1.38777878078144E-17,-1.09743718996384E-46,
-1.));
#1246=DIRECTION('center_axis',(1.,-7.90786835165394E-30,1.38777878078144E-17));
#1247=DIRECTION('ref_axis',(1.38777878078144E-17,-1.09743718996384E-46,
-1.));
#1248=DIRECTION('',(-1.,7.90786835165394E-30,-1.38777878078144E-17));
#1249=DIRECTION('center_axis',(1.,-7.90786835165394E-30,1.38777878078144E-17));
#1250=DIRECTION('ref_axis',(1.38777878078144E-17,-1.09743718996384E-46,
-1.));
#1251=DIRECTION('center_axis',(1.,-7.90786835165394E-30,1.38777878078144E-17));
#1252=DIRECTION('ref_axis',(1.38777878078144E-17,-1.09743718996384E-46,
-1.));
#1253=DIRECTION('center_axis',(-1.38777878078144E-17,-3.94430452610503E-30,
1.));
#1254=DIRECTION('ref_axis',(1.,-7.90786835165394E-30,1.38777878078144E-17));
#1255=DIRECTION('',(1.,-7.90786835165394E-30,1.38777878078144E-17));
#1256=DIRECTION('',(-8.09275762631517E-30,1.,-3.72243739651165E-30));
#1257=DIRECTION('',(-1.,7.90786835165394E-30,-1.38777878078144E-17));
#1258=DIRECTION('',(8.09275762631517E-30,-1.,3.72243739651165E-30));
#1259=DIRECTION('',(1.,-7.90786835165394E-30,1.38777878078144E-17));
#1260=DIRECTION('',(-8.09275762631517E-30,1.,-3.72243739651165E-30));
#1261=DIRECTION('',(-1.,7.90786835165394E-30,-1.38777878078144E-17));
#1262=DIRECTION('',(8.09275762631517E-30,-1.,3.72243739651165E-30));
#1263=DIRECTION('',(8.09275762631517E-30,-1.,3.72243739651165E-30));
#1264=DIRECTION('center_axis',(-1.38777878078144E-17,-3.94430452610503E-30,
1.));
#1265=DIRECTION('ref_axis',(1.,-7.90786835165394E-30,1.38777878078144E-17));
#1266=DIRECTION('',(-8.09275762631517E-30,1.,-3.72243739651165E-30));
#1267=DIRECTION('',(1.,-8.05423902742737E-30,1.04083408558608E-17));
#1268=DIRECTION('',(8.09275762631517E-30,-1.,3.72243739651165E-30));
#1269=DIRECTION('',(8.09275762631517E-30,-1.,3.72243739651165E-30));
#1270=DIRECTION('',(-1.,7.90786835165394E-30,-1.38777878078144E-17));
#1271=DIRECTION('',(-8.09275762631517E-30,1.,-3.72243739651165E-30));
#1272=DIRECTION('',(1.,-7.90786835165394E-30,1.38777878078144E-17));
#1273=DIRECTION('',(8.09275762631517E-30,-1.,3.72243739651165E-30));
#1274=DIRECTION('',(-1.,7.90786835165394E-30,-1.38777878078144E-17));
#1275=DIRECTION('center_axis',(1.,-8.05423902742737E-30,1.38777878078144E-17));
#1276=DIRECTION('ref_axis',(1.38777878078144E-17,3.94430452610503E-30,-1.));
#1277=DIRECTION('',(1.04083408558608E-17,3.77174120308794E-30,-1.));
#1278=DIRECTION('center_axis',(8.09237244032629E-30,-1.,-3.94430452610503E-30));
#1279=DIRECTION('ref_axis',(1.38777878078144E-17,3.94430452610503E-30,-1.));
#1280=DIRECTION('center_axis',(8.09275762631517E-30,-1.,3.72243739651165E-30));
#1281=DIRECTION('ref_axis',(-9.8532293435482E-14,3.72243739651085E-30,1.));
#1282=DIRECTION('center_axis',(1.,-8.05423902742737E-30,1.38777878078144E-17));
#1283=DIRECTION('ref_axis',(1.38777878078144E-17,3.94430452610503E-30,-1.));
#1284=DIRECTION('',(1.04083408558608E-17,3.77174120308794E-30,-1.));
#1285=DIRECTION('center_axis',(-8.09237244032629E-30,1.,3.94430452610503E-30));
#1286=DIRECTION('ref_axis',(-1.38777878078144E-17,-3.94430452610503E-30,
1.));
#1287=DIRECTION('center_axis',(8.09237244032629E-30,-1.,3.72243739651165E-30));
#1288=DIRECTION('ref_axis',(-1.87350135405494E-13,3.72243739651013E-30,
1.));
#1289=DIRECTION('center_axis',(8.09237244032629E-30,-1.,-3.94430452610503E-30));
#1290=DIRECTION('ref_axis',(1.38777878078144E-17,3.94430452610503E-30,-1.));
#1291=DIRECTION('center_axis',(-8.09237244032629E-30,1.,-3.72243739651165E-30));
#1292=DIRECTION('ref_axis',(-1.19040579862585E-13,-3.72243739651261E-30,
-1.));
#1293=DIRECTION('',(1.04083408558608E-17,3.77174120308794E-30,-1.));
#1294=DIRECTION('center_axis',(1.,-8.05423902742737E-30,1.38777878078144E-17));
#1295=DIRECTION('ref_axis',(1.38777878078144E-17,3.94430452610503E-30,-1.));
#1296=DIRECTION('',(1.04083408558608E-17,3.77174120308794E-30,-1.));
#1297=DIRECTION('',(-8.09275762631517E-30,1.,-3.72243739651165E-30));
#1298=DIRECTION('',(8.09275762631517E-30,-1.,3.72243739651165E-30));
#1299=DIRECTION('',(-1.38777878078144E-17,-3.94430452610503E-30,1.));
#1300=DIRECTION('center_axis',(-8.09237244032629E-30,1.,3.94430452610503E-30));
#1301=DIRECTION('ref_axis',(-1.38777878078144E-17,-3.94430452610503E-30,
1.));
#1302=DIRECTION('center_axis',(8.09237244032629E-30,-1.,3.72243739651165E-30));
#1303=DIRECTION('ref_axis',(-9.8532293435482E-14,3.72243739651085E-30,1.));
#1304=DIRECTION('center_axis',(-1.,7.90786835165394E-30,-1.38777878078144E-17));
#1305=DIRECTION('ref_axis',(-1.38777878078144E-17,-3.94430452610503E-30,
1.));
#1306=DIRECTION('',(8.09275762631517E-30,-1.,3.72243739651165E-30));
#1307=DIRECTION('',(1.38777878078144E-17,3.94430452610503E-30,-1.));
#1308=DIRECTION('',(-8.09275762631517E-30,1.,-3.72243739651165E-30));
#1309=DIRECTION('center_axis',(-8.09275762631517E-30,1.,-3.72243739651165E-30));
#1310=DIRECTION('ref_axis',(-3.01247836291004E-59,3.72243739651165E-30,
1.));
#1311=DIRECTION('center_axis',(-8.09275762631517E-30,1.,-3.72243739651165E-30));
#1312=DIRECTION('ref_axis',(-3.01247836291004E-59,3.72243739651165E-30,
1.));
#1313=DIRECTION('center_axis',(1.38777878078144E-17,3.94430452610503E-30,
-1.));
#1314=DIRECTION('ref_axis',(-1.,7.90786835165394E-30,-1.38777878078144E-17));
#1315=DIRECTION('',(-1.,7.90786835165394E-30,-1.38777878078144E-17));
#1316=DIRECTION('center_axis',(-8.09275762631516E-30,1.,3.94430452610503E-30));
#1317=DIRECTION('ref_axis',(-1.38777878078144E-17,-3.94430452610503E-30,
1.));
#1318=DIRECTION('',(-1.,7.90786835165394E-30,-1.38777878078144E-17));
#1319=DIRECTION('center_axis',(-1.38777878078144E-17,-3.94430452610503E-30,
1.));
#1320=DIRECTION('ref_axis',(1.,-7.90786835165394E-30,1.38777878078144E-17));
#1321=DIRECTION('axis',(0.,0.,1.));
#1322=DIRECTION('refdir',(1.,0.,0.));
#1323=DIRECTION('center_axis',(1.,4.14398494273913E-29,6.31088724176809E-30));
#1324=DIRECTION('ref_axis',(0.,-1.7347234759767E-18,-1.));
#1325=DIRECTION('center_axis',(1.,4.14398494273913E-29,6.31088724176809E-30));
#1326=DIRECTION('ref_axis',(6.31088724176809E-30,-1.7347234759767E-18,-1.));
#1327=DIRECTION('center_axis',(4.14398494273913E-29,-1.,-1.20729956438759E-16));
#1328=DIRECTION('ref_axis',(0.,-1.20729956438759E-16,1.));
#1329=DIRECTION('center_axis',(-1.,-4.14398494273913E-29,-6.31088724176809E-30));
#1330=DIRECTION('ref_axis',(6.31088724176809E-30,-1.7347234759767E-18,-1.));
#1331=DIRECTION('center_axis',(-1.,-4.14398494273913E-29,-6.31088724176809E-30));
#1332=DIRECTION('ref_axis',(6.31088724176809E-30,-1.7347234759767E-18,-1.));
#1333=DIRECTION('center_axis',(-6.50810246807336E-30,-1.7347234759767E-18,
-1.));
#1334=DIRECTION('ref_axis',(-1.,-4.14398494273912E-29,6.50810246807336E-30));
#1335=DIRECTION('',(-6.50810246807336E-30,-1.7347234759767E-18,-1.));
#1336=DIRECTION('center_axis',(-1.,-4.14398494273913E-29,-6.31088724176809E-30));
#1337=DIRECTION('ref_axis',(-6.31088724176809E-30,1.7347234759767E-18,1.));
#1338=DIRECTION('center_axis',(1.,4.14398494273913E-29,6.31088724176809E-30));
#1339=DIRECTION('ref_axis',(6.31088724176809E-30,-1.7347234759767E-18,-1.));
#1340=DIRECTION('',(1.,4.14398494273913E-29,6.31088724176809E-30));
#1341=DIRECTION('center_axis',(1.,4.14398494273913E-29,6.31088724176809E-30));
#1342=DIRECTION('ref_axis',(6.31088724176809E-30,-1.7347234759767E-18,-1.));
#1343=DIRECTION('center_axis',(1.,4.14398494273913E-29,6.31088724176809E-30));
#1344=DIRECTION('ref_axis',(6.31088724176809E-30,-1.7347234759767E-18,-1.));
#1345=DIRECTION('',(-1.,-4.14398494273913E-29,-6.31088724176809E-30));
#1346=DIRECTION('',(-1.,-4.14398494273913E-29,-6.31088724176809E-30));
#1347=DIRECTION('center_axis',(1.,4.14398494273913E-29,6.31088724176809E-30));
#1348=DIRECTION('ref_axis',(6.31088724176809E-30,-1.7347234759767E-18,-1.));
#1349=DIRECTION('center_axis',(1.,4.14398494273913E-29,-6.50810246807336E-30));
#1350=DIRECTION('ref_axis',(-6.50810246807336E-30,-1.7347234759767E-18,
-1.));
#1351=DIRECTION('center_axis',(1.,4.14398494273913E-29,-6.50810246807336E-30));
#1352=DIRECTION('ref_axis',(-6.50810246807336E-30,-1.7347234759767E-18,
-1.));
#1353=DIRECTION('center_axis',(1.,4.14398494273913E-29,-6.50810246807336E-30));
#1354=DIRECTION('ref_axis',(-6.50810246807336E-30,-1.7347234759767E-18,
-1.));
#1355=DIRECTION('axis',(0.,0.,1.));
#1356=DIRECTION('refdir',(1.,0.,0.));
#1357=DIRECTION('center_axis',(1.7347234759767E-18,1.,-1.38050658413677E-30));
#1358=DIRECTION('ref_axis',(-4.16000867987644E-29,1.38050658413677E-30,
1.));
#1359=DIRECTION('',(1.7347234759767E-18,1.,-1.38050658413677E-30));
#1360=DIRECTION('center_axis',(1.7347234759767E-18,1.,-1.38050658413677E-30));
#1361=DIRECTION('ref_axis',(-4.16000867987644E-29,1.38050658413677E-30,
1.));
#1362=DIRECTION('',(1.7347234759767E-18,1.,-1.38050658413677E-30));
#1363=DIRECTION('center_axis',(4.15754348954763E-29,4.93038065763134E-30,
-1.));
#1364=DIRECTION('ref_axis',(-1.,1.73472347598838E-18,-4.15754348954763E-29));
#1365=DIRECTION('center_axis',(-4.15754348954763E-29,-4.93038065763134E-30,
1.));
#1366=DIRECTION('ref_axis',(1.,-1.73472347598838E-18,4.15754348954763E-29));
#1367=DIRECTION('',(4.15754348954763E-29,4.93038065763134E-30,-1.));
#1368=DIRECTION('center_axis',(-4.15754348954763E-29,-4.93038065763134E-30,
1.));
#1369=DIRECTION('ref_axis',(1.,-1.73472347597692E-18,4.15754348954763E-29));
#1370=DIRECTION('center_axis',(4.15754348954763E-29,4.93038065763134E-30,
-1.));
#1371=DIRECTION('ref_axis',(-1.,1.73472347598312E-18,-4.15754348954763E-29));
#1372=DIRECTION('center_axis',(-4.15754348954763E-29,-4.93038065763134E-30,
1.));
#1373=DIRECTION('ref_axis',(1.,-1.73472347597692E-18,4.15754348954763E-29));
#1374=DIRECTION('',(-4.15754348954763E-29,-4.93038065763134E-30,1.));
#1375=DIRECTION('center_axis',(-4.15754348954763E-29,-4.93038065763134E-30,
1.));
#1376=DIRECTION('ref_axis',(1.,-1.73472347598312E-18,4.15754348954763E-29));
#1377=DIRECTION('center_axis',(4.1698694411917E-29,-4.93038065763134E-30,
1.));
#1378=DIRECTION('ref_axis',(1.,-1.73472347597692E-18,-4.1698694411917E-29));
#1379=DIRECTION('center_axis',(4.1698694411917E-29,-4.93038065763134E-30,
1.));
#1380=DIRECTION('ref_axis',(1.,-1.73472347597692E-18,-4.1698694411917E-29));
#1381=DIRECTION('axis',(0.,0.,1.));
#1382=DIRECTION('refdir',(1.,0.,0.));
#1383=DIRECTION('center_axis',(-1.06387995116713E-16,-6.73459620742395E-16,
-1.));
#1384=DIRECTION('ref_axis',(-1.,2.27595720048158E-15,1.06387995116711E-16));
#1385=DIRECTION('center_axis',(1.06387995116713E-16,6.73459620742395E-16,
1.));
#1386=DIRECTION('ref_axis',(1.,-2.27595720048158E-15,-1.06387995116711E-16));
#1387=DIRECTION('',(1.06387995116713E-16,6.73459620742395E-16,1.));
#1388=DIRECTION('center_axis',(1.06387995116713E-16,6.73459620742395E-16,
1.));
#1389=DIRECTION('ref_axis',(1.,-2.27595720048158E-15,-1.06387995116711E-16));
#1390=DIRECTION('center_axis',(-1.00785894677507E-16,6.73459620742396E-16,
1.));
#1391=DIRECTION('ref_axis',(1.,-2.27595720048158E-15,1.00785894677509E-16));
#1392=DIRECTION('center_axis',(-1.00785894677507E-16,6.73459620742396E-16,
1.));
#1393=DIRECTION('ref_axis',(1.,-2.27595720048158E-15,1.00785894677509E-16));
#1394=DIRECTION('axis',(0.,0.,1.));
#1395=DIRECTION('refdir',(1.,0.,0.));
#1396=DIRECTION('center_axis',(1.40946282423116E-17,-7.79000143905744E-30,
-1.));
#1397=DIRECTION('ref_axis',(-1.,1.65167752030648E-30,-1.40946282423116E-17));
#1398=DIRECTION('center_axis',(-1.40946282423116E-17,7.79000143905744E-30,
1.));
#1399=DIRECTION('ref_axis',(1.,-1.65167752030648E-30,1.40946282423116E-17));
#1400=DIRECTION('',(-1.40946282423116E-17,7.79000143905744E-30,1.));
#1401=DIRECTION('center_axis',(-1.40946282423116E-17,7.79000143905744E-30,
1.));
#1402=DIRECTION('ref_axis',(1.,-1.65167752030648E-30,1.40946282423116E-17));
#1403=DIRECTION('center_axis',(-1.40946282423116E-17,7.79000143905744E-30,
1.));
#1404=DIRECTION('ref_axis',(1.,-1.65167752030648E-30,1.40946282423116E-17));
#1405=DIRECTION('',(1.40946282423116E-17,-7.79000143905744E-30,-1.));
#1406=DIRECTION('',(-1.40946282423116E-17,7.79000143905744E-30,1.));
#1407=DIRECTION('center_axis',(-1.40946282423114E-17,7.79000143905744E-30,
1.));
#1408=DIRECTION('ref_axis',(1.,-1.65167752030648E-30,1.40946282423114E-17));
#1409=DIRECTION('',(-1.84889274661175E-30,1.,7.29696337329436E-30));
#1410=DIRECTION('',(1.,-1.65167752030648E-30,1.40946282423114E-17));
#1411=DIRECTION('',(-1.84889274661175E-30,1.,7.29696337329436E-30));
#1412=DIRECTION('center_axis',(-1.40946282423114E-17,7.79000143905744E-30,
1.));
#1413=DIRECTION('ref_axis',(1.,-1.65167752030648E-30,1.40946282423114E-17));
#1414=DIRECTION('center_axis',(1.,-1.7009813268828E-30,1.40946282423116E-17));
#1415=DIRECTION('ref_axis',(1.40946282423116E-17,-7.79000143905744E-30,
-1.));
#1416=DIRECTION('center_axis',(1.,-1.7009813268828E-30,1.04083408558607E-17));
#1417=DIRECTION('ref_axis',(1.04083408558607E-17,-1.77043934396503E-47,
-1.));
#1418=DIRECTION('',(1.04083408558609E-17,-7.69139382590482E-30,-1.));
#1419=DIRECTION('center_axis',(-1.,1.7009813268828E-30,-1.40946282423116E-17));
#1420=DIRECTION('ref_axis',(-1.40946282423116E-17,7.79000143905744E-30,
1.));
#1421=DIRECTION('',(1.04083408558609E-17,-7.69139382590482E-30,-1.));
#1422=DIRECTION('center_axis',(-1.,1.7009813268828E-30,-1.04083408558607E-17));
#1423=DIRECTION('ref_axis',(-1.04083408558607E-17,1.77043934396503E-47,
1.));
#1424=DIRECTION('center_axis',(-1.84889274661175E-30,1.,-7.79000143905744E-30));
#1425=DIRECTION('ref_axis',(-1.40946282423116E-17,7.79000143905744E-30,
1.));
#1426=DIRECTION('',(1.,-1.65167752030648E-30,1.40946282423114E-17));
#1427=DIRECTION('center_axis',(1.,-1.65167752030648E-30,1.40946282423114E-17));
#1428=DIRECTION('ref_axis',(1.40946282423114E-17,-2.32797806249026E-47,
-1.));
#1429=DIRECTION('axis',(0.,0.,1.));
#1430=DIRECTION('refdir',(1.,0.,0.));
#1431=DIRECTION('center_axis',(1.,-3.57452597678267E-31,1.04083408558607E-17));
#1432=DIRECTION('ref_axis',(1.04083408558607E-17,1.47911419728938E-31,-1.));
#1433=DIRECTION('',(1.04083408558607E-17,1.47911419728938E-31,-1.));
#1434=DIRECTION('',(3.6977854932235E-31,-1.,0.));
#1435=DIRECTION('',(1.04083408558607E-17,1.47911419728938E-31,-1.));
#1436=DIRECTION('',(-3.6977854932235E-31,1.,0.));
#1437=DIRECTION('center_axis',(-3.69778549322349E-31,1.,1.47911419728938E-31));
#1438=DIRECTION('ref_axis',(-1.04083408558607E-17,-1.47911419728938E-31,
1.));
#1439=DIRECTION('center_axis',(3.69778549322349E-31,-1.,0.));
#1440=DIRECTION('ref_axis',(-5.46944702155759E-62,-2.02248418522701E-92,
1.));
#1441=DIRECTION('',(1.04083408558607E-17,1.47911419728938E-31,-1.));
#1442=DIRECTION('center_axis',(3.69778549322349E-31,-1.,0.));
#1443=DIRECTION('ref_axis',(-5.46944702155759E-62,-2.02248418522701E-92,
1.));
#1444=DIRECTION('center_axis',(-1.,3.57452597678267E-31,-1.04083408558607E-17));
#1445=DIRECTION('ref_axis',(-1.04083408558607E-17,-1.47911419728938E-31,
1.));
#1446=DIRECTION('',(-3.6977854932235E-31,1.,0.));
#1447=DIRECTION('',(1.04083408558607E-17,1.47911419728938E-31,-1.));
#1448=DIRECTION('',(3.6977854932235E-31,-1.,0.));
#1449=DIRECTION('center_axis',(3.69778549322349E-31,-1.,-1.47911419728938E-31));
#1450=DIRECTION('ref_axis',(1.04083408558607E-17,1.47911419728938E-31,-1.));
#1451=DIRECTION('center_axis',(-3.69778549322349E-31,1.,0.));
#1452=DIRECTION('ref_axis',(-4.16507106582027E-13,-1.54015393654351E-43,
-1.));
#1453=DIRECTION('center_axis',(-3.69778549322349E-31,1.,0.));
#1454=DIRECTION('ref_axis',(0.,0.,-1.));
#1455=DIRECTION('center_axis',(-3.69778549322349E-31,1.,0.));
#1456=DIRECTION('ref_axis',(1.66655918373688E-13,6.16257837322063E-44,-1.));
#1457=DIRECTION('center_axis',(3.69778549322349E-31,-1.,0.));
#1458=DIRECTION('ref_axis',(1.10899837782601E-13,4.1008381135334E-44,1.));
#1459=DIRECTION('',(0.,0.,1.));
#1460=DIRECTION('',(1.,0.,0.));
#1461=DIRECTION('',(-0.0159962732484479,1.87940168220745E-16,0.999872051435663));
#1462=DIRECTION('',(0.999872051435663,2.35080123756906E-16,0.0159962732484479));
#1463=DIRECTION('',(-0.999986830341514,-0.00513216752772264,1.34025299928118E-15));
#1464=DIRECTION('',(1.33981051673149E-15,8.96555683642807E-17,1.));
#1465=DIRECTION('',(1.33982581559821E-15,8.66746319138549E-17,1.));
#1466=DIRECTION('',(0.00513216752772262,-0.999986830341514,7.97972798949355E-17));
#1467=DIRECTION('',(0.999986830341514,0.005132167527723,-1.50112539712064E-15));
#1468=DIRECTION('',(0.00293547096689554,-0.5719673591884,0.82027112775792));
#1469=DIRECTION('',(-0.999872051435663,-3.44857200412933E-16,-0.0159962732484479));
#1470=DIRECTION('',(-0.0159962732484479,-2.41864082158329E-16,0.999872051435663));
#1471=DIRECTION('',(-0.999872051435663,0.,-0.0159962732484485));
#1472=DIRECTION('',(-0.0159962732484485,0.,0.999872051435663));
#1473=DIRECTION('',(-0.00130713958206112,-0.999999145692692,-2.74063052618212E-16));
#1474=DIRECTION('',(-0.999999145692692,0.00130713958206112,-4.20995138881959E-16));
#1475=DIRECTION('',(0.,0.,1.));
#1476=DIRECTION('',(1.22464679914735E-16,-1.,0.));
#1477=DIRECTION('',(0.,-1.,0.));
#1478=DIRECTION('',(1.,0.,0.));
#1479=DIRECTION('',(0.,0.,1.));
#1480=DIRECTION('',(1.,0.,0.));
#1481=DIRECTION('',(0.999999145692692,-0.00130713958206112,4.3689951285086E-16));
#1482=DIRECTION('',(-0.00130713958206112,-0.999999145692692,-2.02685302490279E-16));
#1483=DIRECTION('',(0.999999145692692,-0.00130713958205944,1.20919539802822E-16));
#1484=DIRECTION('',(0.00130713958205944,0.999999145692692,6.00368489128965E-17));
#1485=CARTESIAN_POINT('',(0.,0.,0.));
#1486=CARTESIAN_POINT('',(0.,0.,0.));
#1487=CARTESIAN_POINT('Origin',(-40.,55.,55.));
#1488=CARTESIAN_POINT('',(-40.,55.,70.));
#1489=CARTESIAN_POINT('Origin',(-40.,55.,55.));
#1490=CARTESIAN_POINT('',(-40.,-55.,70.));
#1491=CARTESIAN_POINT('',(-40.,55.,70.));
#1492=CARTESIAN_POINT('Origin',(-40.,-55.,55.));
#1493=CARTESIAN_POINT('Origin',(-40.,55.,55.));
#1494=CARTESIAN_POINT('',(-40.,-55.,80.));
#1495=CARTESIAN_POINT('Origin',(-40.,-55.,55.));
#1496=CARTESIAN_POINT('',(-40.,55.,80.));
#1497=CARTESIAN_POINT('',(-40.,55.,80.));
#1498=CARTESIAN_POINT('Origin',(-40.,55.,55.));
#1499=CARTESIAN_POINT('',(-24.9999999999999,0.,75.));
#1500=CARTESIAN_POINT('Ctrl Pts',(-25.,2.77555756156289E-16,35.));
#1501=CARTESIAN_POINT('Ctrl Pts',(-25.,-1.24361617380203,35.));
#1502=CARTESIAN_POINT('Ctrl Pts',(-24.9052472768386,-2.5300488634612,35.069860816135));
#1503=CARTESIAN_POINT('Ctrl Pts',(-24.5112512498491,-5.08635930324528,35.3744893013021));
#1504=CARTESIAN_POINT('Ctrl Pts',(-24.2120237975874,-6.35622364547916,35.6093899705556));
#1505=CARTESIAN_POINT('Ctrl Pts',(-23.4403103697305,-8.78494699666433,36.2641295306962));
#1506=CARTESIAN_POINT('Ctrl Pts',(-22.9672284001806,-9.94593352803297,36.6853433784887));
#1507=CARTESIAN_POINT('Ctrl Pts',(-21.9190504199837,-12.0818210937726,37.7193397258191));
#1508=CARTESIAN_POINT('Ctrl Pts',(-21.3446200198761,-13.0565914520077,38.3330665709257));
#1509=CARTESIAN_POINT('Ctrl Pts',(-20.2669777826776,-14.6650944479835,39.6303382528525));
#1510=CARTESIAN_POINT('Ctrl Pts',(-19.7036276546287,-15.410730934833,40.3700017631622));
#1511=CARTESIAN_POINT('Ctrl Pts',(-18.6105706812708,-16.7143714911116,42.0203271120065));
#1512=CARTESIAN_POINT('Ctrl Pts',(-18.0833825531526,-17.2737939159714,42.9315354562001));
#1513=CARTESIAN_POINT('Ctrl Pts',(-16.8688323188826,-18.4830916199472,45.3606359247402));
#1514=CARTESIAN_POINT('Ctrl Pts',(-16.1653056845286,-19.079941900497,47.1971676511035));
#1515=CARTESIAN_POINT('Ctrl Pts',(-15.2297367266376,-19.8347251545665,51.0743159129527));
#1516=CARTESIAN_POINT('Ctrl Pts',(-15.,-20.,53.1140556509152));
#1517=CARTESIAN_POINT('Ctrl Pts',(-15.,-20.,56.8859443490849));
#1518=CARTESIAN_POINT('Ctrl Pts',(-15.2297367266376,-19.8347251545665,58.9256840870473));
#1519=CARTESIAN_POINT('Ctrl Pts',(-16.1653056845286,-19.079941900497,62.8028323488965));
#1520=CARTESIAN_POINT('Ctrl Pts',(-16.8688323188826,-18.4830916199472,64.6393640752598));
#1521=CARTESIAN_POINT('Ctrl Pts',(-18.0833825531526,-17.2737939159714,67.0684645437999));
#1522=CARTESIAN_POINT('Ctrl Pts',(-18.6105706812708,-16.7143714911116,67.9796728879935));
#1523=CARTESIAN_POINT('Ctrl Pts',(-19.7036276546287,-15.410730934833,69.6299982368378));
#1524=CARTESIAN_POINT('Ctrl Pts',(-20.2669777826776,-14.6650944479835,70.3696617471475));
#1525=CARTESIAN_POINT('Ctrl Pts',(-21.3446200198761,-13.0565914520077,71.6669334290743));
#1526=CARTESIAN_POINT('Ctrl Pts',(-21.9190504199837,-12.0818210937726,72.2806602741809));
#1527=CARTESIAN_POINT('Ctrl Pts',(-22.9672284001806,-9.94593352803297,73.3146566215113));
#1528=CARTESIAN_POINT('Ctrl Pts',(-23.4403103697305,-8.78494699666433,73.7358704693038));
#1529=CARTESIAN_POINT('Ctrl Pts',(-24.2120237975874,-6.35622364547916,74.3906100294445));
#1530=CARTESIAN_POINT('Ctrl Pts',(-24.5112512498491,-5.08635930324528,74.6255106986979));
#1531=CARTESIAN_POINT('Ctrl Pts',(-24.9052472768386,-2.53004886346119,74.930139183865));
#1532=CARTESIAN_POINT('Ctrl Pts',(-25.,-1.24361617380203,75.));
#1533=CARTESIAN_POINT('Ctrl Pts',(-25.,1.24361617380203,75.));
#1534=CARTESIAN_POINT('Ctrl Pts',(-24.9052472768386,2.53004886346119,74.930139183865));
#1535=CARTESIAN_POINT('Ctrl Pts',(-24.5112512498491,5.08635930324528,74.6255106986979));
#1536=CARTESIAN_POINT('Ctrl Pts',(-24.2120237975874,6.35622364547916,74.3906100294445));
#1537=CARTESIAN_POINT('Ctrl Pts',(-23.4403103697305,8.78494699666433,73.7358704693038));
#1538=CARTESIAN_POINT('Ctrl Pts',(-22.9672284001806,9.94593352803297,73.3146566215113));
#1539=CARTESIAN_POINT('Ctrl Pts',(-21.9190504199837,12.0818210937726,72.2806602741809));
#1540=CARTESIAN_POINT('Ctrl Pts',(-21.3446200198761,13.0565914520077,71.6669334290743));
#1541=CARTESIAN_POINT('Ctrl Pts',(-20.2669777826776,14.6650944479835,70.3696617471475));
#1542=CARTESIAN_POINT('Ctrl Pts',(-19.7036276546287,15.410730934833,69.6299982368378));
#1543=CARTESIAN_POINT('Ctrl Pts',(-18.6105706812708,16.7143714911116,67.9796728879935));
#1544=CARTESIAN_POINT('Ctrl Pts',(-18.0833825531526,17.2737939159714,67.0684645437999));
#1545=CARTESIAN_POINT('Ctrl Pts',(-16.8688323188826,18.4830916199472,64.6393640752599));
#1546=CARTESIAN_POINT('Ctrl Pts',(-16.1653056845287,19.079941900497,62.8028323488965));
#1547=CARTESIAN_POINT('Ctrl Pts',(-15.2297367266376,19.8347251545665,58.9256840870473));
#1548=CARTESIAN_POINT('Ctrl Pts',(-15.,20.,56.8859443490849));
#1549=CARTESIAN_POINT('Ctrl Pts',(-15.,20.,53.1140556509151));
#1550=CARTESIAN_POINT('Ctrl Pts',(-15.2297367266376,19.8347251545665,51.0743159129527));
#1551=CARTESIAN_POINT('Ctrl Pts',(-16.1653056845287,19.079941900497,47.1971676511035));
#1552=CARTESIAN_POINT('Ctrl Pts',(-16.8688323188826,18.4830916199472,45.3606359247402));
#1553=CARTESIAN_POINT('Ctrl Pts',(-18.0833825531526,17.2737939159714,42.9315354562001));
#1554=CARTESIAN_POINT('Ctrl Pts',(-18.6105706812708,16.7143714911116,42.0203271120065));
#1555=CARTESIAN_POINT('Ctrl Pts',(-19.7036276546287,15.410730934833,40.3700017631622));
#1556=CARTESIAN_POINT('Ctrl Pts',(-20.2669777826776,14.6650944479835,39.6303382528525));
#1557=CARTESIAN_POINT('Ctrl Pts',(-21.3446200198761,13.0565914520077,38.3330665709257));
#1558=CARTESIAN_POINT('Ctrl Pts',(-21.9190504199837,12.0818210937726,37.7193397258191));
#1559=CARTESIAN_POINT('Ctrl Pts',(-22.9672284001806,9.94593352803297,36.6853433784887));
#1560=CARTESIAN_POINT('Ctrl Pts',(-23.4403103697305,8.78494699666433,36.2641295306962));
#1561=CARTESIAN_POINT('Ctrl Pts',(-24.2120237975874,6.35622364547916,35.6093899705556));
#1562=CARTESIAN_POINT('Ctrl Pts',(-24.5112512498491,5.08635930324528,35.3744893013021));
#1563=CARTESIAN_POINT('Ctrl Pts',(-24.9052472768386,2.53004886346119,35.069860816135));
#1564=CARTESIAN_POINT('Ctrl Pts',(-25.,1.24361617380203,35.));
#1565=CARTESIAN_POINT('Ctrl Pts',(-25.,-2.77555756156289E-16,35.));
#1566=CARTESIAN_POINT('Origin',(0.,0.,110.));
#1567=CARTESIAN_POINT('',(15.,-1.83697019872103E-15,110.));
#1568=CARTESIAN_POINT('Origin',(0.,0.,110.));
#1569=CARTESIAN_POINT('',(15.,-1.83697019872103E-15,0.));
#1570=CARTESIAN_POINT('',(15.,-1.83697019872103E-15,110.));
#1571=CARTESIAN_POINT('Origin',(0.,0.,0.));
#1572=CARTESIAN_POINT('Origin',(0.,0.,110.));
#1573=CARTESIAN_POINT('',(25.,-3.06161699786838E-15,0.));
#1574=CARTESIAN_POINT('Origin',(0.,0.,0.));
#1575=CARTESIAN_POINT('',(25.,-3.06161699786838E-15,110.));
#1576=CARTESIAN_POINT('',(25.,-3.06161699786838E-15,110.));
#1577=CARTESIAN_POINT('Origin',(0.,0.,110.));
#1578=CARTESIAN_POINT('Origin',(0.,0.,110.));
#1579=CARTESIAN_POINT('Origin',(0.,0.,0.));
#1580=CARTESIAN_POINT('Origin',(-40.,55.,55.));
#1581=CARTESIAN_POINT('Origin',(-40.,-55.,55.));
#1582=CARTESIAN_POINT('',(0.,0.,0.));
#1583=CARTESIAN_POINT('Origin',(60.0822225038815,-312.623333755829,0.));
#1584=CARTESIAN_POINT('',(60.0822225038815,-107.623333755829,-15.0000000000001));
#1585=CARTESIAN_POINT('Origin',(60.0822225038811,-107.623333755829,2.22044604925031E-13));
#1586=CARTESIAN_POINT('',(60.0822225038815,-82.6233337558287,-15.0000000000001));
#1587=CARTESIAN_POINT('',(60.0822225038815,-312.623333755829,-15.0000000000001));
#1588=CARTESIAN_POINT('Origin',(60.0822225038811,-82.6233337558288,3.33066907387547E-13));
#1589=CARTESIAN_POINT('Origin',(60.0822225038815,-312.623333755829,0.));
#1590=CARTESIAN_POINT('',(60.0822225038815,27.3766662441712,-15.0000000000001));
#1591=CARTESIAN_POINT('Origin',(60.0822225038811,27.3766662441712,5.55111512312578E-13));
#1592=CARTESIAN_POINT('',(60.0822225038815,52.3766662441712,-15.0000000000001));
#1593=CARTESIAN_POINT('',(60.0822225038815,-312.623333755829,-15.0000000000001));
#1594=CARTESIAN_POINT('Origin',(60.0822225038811,52.3766662441712,4.44089209850063E-13));
#1595=CARTESIAN_POINT('Origin',(-34.9177774961142,-27.6233337558284,-2.22044604925031E-13));
#1596=CARTESIAN_POINT('',(-89.917777496118,-4.71045528104919,9.99999999999956));
#1597=CARTESIAN_POINT('',(-89.9177774961188,-4.71045528104924,-10.0000000000011));
#1598=CARTESIAN_POINT('Origin',(-89.9177774961135,-27.6233337558284,-2.22044604925031E-13));
#1599=CARTESIAN_POINT('',(-9.91777749611433,-4.71045528104919,9.99999999999979));
#1600=CARTESIAN_POINT('',(-34.9177774961102,-4.71045528104919,9.99999999999934));
#1601=CARTESIAN_POINT('',(-9.91777749611433,-4.71045528104919,-10.0000000000002));
#1602=CARTESIAN_POINT('Origin',(-9.91777749611433,-27.6233337558284,7.7715611723761E-13));
#1603=CARTESIAN_POINT('',(-34.9177774961142,-4.71045528104919,-10.));
#1604=CARTESIAN_POINT('Origin',(-34.9177774961142,-27.6233337558284,-2.22044604925031E-13));
#1605=CARTESIAN_POINT('',(-34.9177774961142,-27.6233337558284,44.9999999999998));
#1606=CARTESIAN_POINT('',(-34.9177774961102,-27.6233337558284,-45.0000000000014));
#1607=CARTESIAN_POINT('Origin',(-34.9177774961142,-27.6233337558284,-2.22044604925031E-13));
#1608=CARTESIAN_POINT('',(-89.9177774961135,-27.6233337558284,45.0000000000001));
#1609=CARTESIAN_POINT('',(-34.9177774961142,-27.6233337558284,45.0000000000001));
#1610=CARTESIAN_POINT('Origin',(-89.9177774961135,-27.6233337558284,-2.22044604925031E-13));
#1611=CARTESIAN_POINT('Origin',(-34.9177774961142,-27.6233337558284,-2.22044604925031E-13));
#1612=CARTESIAN_POINT('Origin',(8.88178419700125E-13,0.,44.9999999999998));
#1613=CARTESIAN_POINT('',(-34.9177774961142,-107.623333755829,44.9999999999999));
#1614=CARTESIAN_POINT('',(60.0822225038895,-107.623333755829,44.9999999999998));
#1615=CARTESIAN_POINT('',(-34.9177774961142,-107.623333755829,44.9999999999999));
#1616=CARTESIAN_POINT('',(60.0822225038895,-82.6233337558287,44.9999999999998));
#1617=CARTESIAN_POINT('',(60.08222250389,-312.623333755829,45.0000000000001));
#1618=CARTESIAN_POINT('',(-9.91777749611789,-82.6233337558287,44.9999999999999));
#1619=CARTESIAN_POINT('',(105.082222503891,-82.6233337558287,45.0000000000001));
#1620=CARTESIAN_POINT('',(-9.91777749611789,27.3766662441716,44.9999999999998));
#1621=CARTESIAN_POINT('',(-9.91777749611789,27.3766662441716,44.9999999999998));
#1622=CARTESIAN_POINT('',(60.0822225038855,27.3766662441712,45.));
#1623=CARTESIAN_POINT('',(-9.91777749611789,27.3766662441716,44.9999999999998));
#1624=CARTESIAN_POINT('',(60.0822225038855,52.3766662441712,45.));
#1625=CARTESIAN_POINT('',(60.08222250389,-312.623333755829,45.0000000000001));
#1626=CARTESIAN_POINT('',(-34.9177774961142,52.3766662441716,44.9999999999998));
#1627=CARTESIAN_POINT('',(105.08222250389,52.3766662441715,44.9999999999996));
#1628=CARTESIAN_POINT('',(-34.9177774961142,52.3766662441716,44.9999999999998));
#1629=CARTESIAN_POINT('',(-34.9177774961142,52.3766662441716,44.9999999999998));
#1630=CARTESIAN_POINT('Origin',(-8.43769498715119E-12,0.,-45.0000000000007));
#1631=CARTESIAN_POINT('',(60.0822225038864,-107.623333755829,-45.0000000000001));
#1632=CARTESIAN_POINT('',(60.0822225038864,-82.6233337558288,-45.0000000000001));
#1633=CARTESIAN_POINT('',(60.0822225038864,0.,-45.000000000001));
#1634=CARTESIAN_POINT('',(-34.9177774961102,-107.623333755829,-45.000000000001));
#1635=CARTESIAN_POINT('',(15.0822225038811,-107.623333755829,-45.0000000000004));
#1636=CARTESIAN_POINT('',(-34.9177774961102,-82.623333755829,-45.0000000000012));
#1637=CARTESIAN_POINT('',(-34.9177774961102,52.3766662441717,-45.0000000000012));
#1638=CARTESIAN_POINT('',(-34.9177774961102,-82.623333755829,-45.0000000000012));
#1639=CARTESIAN_POINT('',(60.0822225038864,52.3766662441712,-45.000000000001));
#1640=CARTESIAN_POINT('',(105.082222503885,52.3766662441712,-45.000000000001));
#1641=CARTESIAN_POINT('',(60.0822225038864,27.3766662441712,-45.000000000001));
#1642=CARTESIAN_POINT('',(60.0822225038864,0.,-45.000000000001));
#1643=CARTESIAN_POINT('',(-9.91777749611433,27.3766662441716,-45.0000000000004));
#1644=CARTESIAN_POINT('',(-9.91777749611433,27.3766662441716,-45.0000000000004));
#1645=CARTESIAN_POINT('',(-9.91777749611034,-82.6233337558288,-45.000000000001));
#1646=CARTESIAN_POINT('',(-9.91777749611433,27.3766662441716,-45.0000000000004));
#1647=CARTESIAN_POINT('',(105.082222503886,-82.6233337558288,-45.0000000000004));
#1648=CARTESIAN_POINT('Origin',(-34.9177774961142,-82.6233337558288,44.9999999999998));
#1649=CARTESIAN_POINT('',(-34.9177774961142,52.3766662441716,44.9999999999998));
#1650=CARTESIAN_POINT('Origin',(105.08222250389,52.3766662441715,44.9999999999996));
#1651=CARTESIAN_POINT('Origin',(60.0822225038811,52.3766662441712,4.44089209850063E-13));
#1652=CARTESIAN_POINT('Origin',(-34.9177774961142,-82.6233337558288,44.9999999999998));
#1653=CARTESIAN_POINT('',(-34.9177774961142,-107.623333755829,44.9999999999999));
#1654=CARTESIAN_POINT('Origin',(15.0822225038874,-107.623333755829,45.));
#1655=CARTESIAN_POINT('Origin',(60.0822225038811,-107.623333755829,2.22044604925031E-13));
#1656=CARTESIAN_POINT('Origin',(105.082222503891,-82.6233337558287,45.0000000000001));
#1657=CARTESIAN_POINT('Origin',(60.0822225038811,-82.6233337558288,3.33066907387547E-13));
#1658=CARTESIAN_POINT('',(-9.91777749611789,-82.6233337558287,44.9999999999999));
#1659=CARTESIAN_POINT('Origin',(-9.91777749611789,27.3766662441716,44.9999999999998));
#1660=CARTESIAN_POINT('',(-9.91777749611789,27.3766662441716,44.9999999999998));
#1661=CARTESIAN_POINT('',(-9.91777749611433,7.3766662441716,-10.0000000000002));
#1662=CARTESIAN_POINT('',(-9.91777749611567,27.3766662441716,-10.0000000000002));
#1663=CARTESIAN_POINT('',(-9.91777749611433,7.3766662441716,9.99999999999979));
#1664=CARTESIAN_POINT('',(-9.91777749611433,27.3766662441716,9.99999999999979));
#1665=CARTESIAN_POINT('',(-9.91777749611789,7.3766662441716,44.9999999999998));
#1666=CARTESIAN_POINT('Origin',(-9.91777749611789,27.3766662441716,44.9999999999998));
#1667=CARTESIAN_POINT('Origin',(60.0822225038811,27.3766662441712,5.55111512312578E-13));
#1668=CARTESIAN_POINT('Origin',(-89.917777496114,3.88578058618805E-13,-2.22044604925031E-13));
#1669=CARTESIAN_POINT('',(-89.9177774961188,7.37666624417127,-10.0000000000011));
#1670=CARTESIAN_POINT('',(-89.9177774961188,7.37666624417127,-10.0000000000011));
#1671=CARTESIAN_POINT('',(-89.917777496118,7.3766662441716,9.99999999999956));
#1672=CARTESIAN_POINT('',(-89.9177774961135,7.37666624417133,-2.22044604925031E-13));
#1673=CARTESIAN_POINT('',(-89.917777496118,7.3766662441716,9.99999999999956));
#1674=CARTESIAN_POINT('Origin',(60.0822225038815,-312.623333755829,0.));
#1675=CARTESIAN_POINT('Origin',(60.0822225038815,-312.623333755829,0.));
#1676=CARTESIAN_POINT('Origin',(275.082222503884,7.37666624417121,-10.0000000000003));
#1677=CARTESIAN_POINT('',(275.082222503884,7.37666624417121,-10.0000000000003));
#1678=CARTESIAN_POINT('Origin',(275.082222503886,7.37666624417121,7.7715611723761E-13));
#1679=CARTESIAN_POINT('',(275.082222503887,7.37666624417121,9.9999999999999));
#1680=CARTESIAN_POINT('Origin',(275.082222503887,7.37666624417121,9.9999999999999));
#1681=CARTESIAN_POINT('',(0.,0.,0.));
#1682=CARTESIAN_POINT('Origin',(2.5,0.,0.));
#1683=CARTESIAN_POINT('',(12.5,-1.81094934658102E-15,15.0000000000004));
#1684=CARTESIAN_POINT('Origin',(12.5,0.,4.44089209850063E-13));
#1685=CARTESIAN_POINT('',(2.5,-3.01824891096896E-15,25.));
#1686=CARTESIAN_POINT('Origin',(2.5,-1.81094934658138E-15,15.));
#1687=CARTESIAN_POINT('',(2.5,3.01824891096855E-15,-25.));
#1688=CARTESIAN_POINT('Origin',(2.5,0.,0.));
#1689=CARTESIAN_POINT('Origin',(2.5,0.,0.));
#1690=CARTESIAN_POINT('Origin',(-166.25,0.,172.5));
#1691=CARTESIAN_POINT('',(-163.75,1.86299093907171E-15,15.000000000004));
#1692=CARTESIAN_POINT('',(-168.75,-9.74863612329683E-16,15.000000000004));
#1693=CARTESIAN_POINT('Ctrl Pts',(-163.75,-1.38777878078145E-16,15.000000000004));
#1694=CARTESIAN_POINT('Ctrl Pts',(-163.75,-0.314532953903506,15.000000000004));
#1695=CARTESIAN_POINT('Ctrl Pts',(-163.8129794775,-0.649633350162397,14.9891013758676));
#1696=CARTESIAN_POINT('Ctrl Pts',(-164.068297410941,-1.26541151060516,14.9497129490472));
#1697=CARTESIAN_POINT('Ctrl Pts',(-164.260603678422,-1.54613758435443,14.9217716767288));
#1698=CARTESIAN_POINT('Ctrl Pts',(-164.703868335279,-1.98940224121134,14.8691658402804));
#1699=CARTESIAN_POINT('Ctrl Pts',(-164.984591867622,-2.18170386550857,14.8410532029514));
#1700=CARTESIAN_POINT('Ctrl Pts',(-165.600361297578,-2.43701842756375,14.8012713411856));
#1701=CARTESIAN_POINT('Ctrl Pts',(-165.935458645045,-2.5,14.790199457753));
#1702=CARTESIAN_POINT('Ctrl Pts',(-166.564541354955,-2.5,14.790199457753));
#1703=CARTESIAN_POINT('Ctrl Pts',(-166.899638702422,-2.43701842756377,14.8012713411856));
#1704=CARTESIAN_POINT('Ctrl Pts',(-167.515408132377,-2.1817038655086,14.8410532029514));
#1705=CARTESIAN_POINT('Ctrl Pts',(-167.796131664721,-1.98940224121134,14.8691658402804));
#1706=CARTESIAN_POINT('Ctrl Pts',(-168.239396321578,-1.54613758435443,14.9217716767288));
#1707=CARTESIAN_POINT('Ctrl Pts',(-168.431702589059,-1.26541151060517,14.9497129490472));
#1708=CARTESIAN_POINT('Ctrl Pts',(-168.6870205225,-0.649633350162398,14.9891013758676));
#1709=CARTESIAN_POINT('Ctrl Pts',(-168.75,-0.314532953903508,15.000000000004));
#1710=CARTESIAN_POINT('Ctrl Pts',(-168.75,-1.17961196366423E-15,15.000000000004));
#1711=CARTESIAN_POINT('',(-163.75,-2.60207403499523E-17,-14.999999999996));
#1712=CARTESIAN_POINT('',(-163.75,-3.06161699786735E-16,172.5));
#1713=CARTESIAN_POINT('Ctrl Pts',(-166.25,2.5,-14.790199457745));
#1714=CARTESIAN_POINT('Ctrl Pts',(-166.564541354955,2.5,-14.790199457745));
#1715=CARTESIAN_POINT('Ctrl Pts',(-166.899638702422,2.43701842756377,-14.8012713411776));
#1716=CARTESIAN_POINT('Ctrl Pts',(-167.515408132377,2.1817038655086,-14.8410532029434));
#1717=CARTESIAN_POINT('Ctrl Pts',(-167.796131664721,1.98940224121134,-14.8691658402724));
#1718=CARTESIAN_POINT('Ctrl Pts',(-168.239396321578,1.54613758435443,-14.9217716767208));
#1719=CARTESIAN_POINT('Ctrl Pts',(-168.431702589059,1.26541151060516,-14.9497129490392));
#1720=CARTESIAN_POINT('Ctrl Pts',(-168.6870205225,0.649633350162396,-14.9891013758596));
#1721=CARTESIAN_POINT('Ctrl Pts',(-168.75,0.314532953903506,-14.999999999996));
#1722=CARTESIAN_POINT('Ctrl Pts',(-168.75,-0.314532953903507,-14.999999999996));
#1723=CARTESIAN_POINT('Ctrl Pts',(-168.6870205225,-0.649633350162412,-14.9891013758596));
#1724=CARTESIAN_POINT('Ctrl Pts',(-168.431702589059,-1.26541151060518,-14.9497129490392));
#1725=CARTESIAN_POINT('Ctrl Pts',(-168.239396321578,-1.54613758435443,-14.9217716767208));
#1726=CARTESIAN_POINT('Ctrl Pts',(-167.796131664721,-1.98940224121134,-14.8691658402724));
#1727=CARTESIAN_POINT('Ctrl Pts',(-167.515408132377,-2.18170386550861,-14.8410532029434));
#1728=CARTESIAN_POINT('Ctrl Pts',(-166.899638702422,-2.43701842756378,-14.8012713411776));
#1729=CARTESIAN_POINT('Ctrl Pts',(-166.564541354955,-2.5,-14.790199457745));
#1730=CARTESIAN_POINT('Ctrl Pts',(-165.935458645045,-2.5,-14.790199457745));
#1731=CARTESIAN_POINT('Ctrl Pts',(-165.600361297578,-2.43701842756375,-14.8012713411776));
#1732=CARTESIAN_POINT('Ctrl Pts',(-164.984591867622,-2.18170386550857,-14.8410532029434));
#1733=CARTESIAN_POINT('Ctrl Pts',(-164.703868335279,-1.98940224121134,-14.8691658402724));
#1734=CARTESIAN_POINT('Ctrl Pts',(-164.260603678422,-1.54613758435443,-14.9217716767208));
#1735=CARTESIAN_POINT('Ctrl Pts',(-164.068297410941,-1.26541151060517,-14.9497129490392));
#1736=CARTESIAN_POINT('Ctrl Pts',(-163.8129794775,-0.649633350162397,-14.9891013758596));
#1737=CARTESIAN_POINT('Ctrl Pts',(-163.75,-0.314532953903507,-14.999999999996));
#1738=CARTESIAN_POINT('Ctrl Pts',(-163.75,0.314532953903505,-14.999999999996));
#1739=CARTESIAN_POINT('Ctrl Pts',(-163.8129794775,0.649633350162396,-14.9891013758596));
#1740=CARTESIAN_POINT('Ctrl Pts',(-164.068297410941,1.26541151060516,-14.9497129490392));
#1741=CARTESIAN_POINT('Ctrl Pts',(-164.260603678422,1.54613758435443,-14.9217716767208));
#1742=CARTESIAN_POINT('Ctrl Pts',(-164.703868335279,1.98940224121134,-14.8691658402724));
#1743=CARTESIAN_POINT('Ctrl Pts',(-164.984591867623,2.1817038655086,-14.8410532029434));
#1744=CARTESIAN_POINT('Ctrl Pts',(-165.600361297578,2.43701842756377,-14.8012713411776));
#1745=CARTESIAN_POINT('Ctrl Pts',(-165.935458645045,2.5,-14.790199457745));
#1746=CARTESIAN_POINT('Ctrl Pts',(-166.25,2.5,-14.790199457745));
#1747=CARTESIAN_POINT('Ctrl Pts',(-168.75,-6.93889390390723E-17,15.000000000004));
#1748=CARTESIAN_POINT('Ctrl Pts',(-168.75,0.314532953903506,15.000000000004));
#1749=CARTESIAN_POINT('Ctrl Pts',(-168.6870205225,0.649633350162395,14.9891013758676));
#1750=CARTESIAN_POINT('Ctrl Pts',(-168.431702589059,1.26541151060516,14.9497129490472));
#1751=CARTESIAN_POINT('Ctrl Pts',(-168.239396321578,1.54613758435443,14.9217716767288));
#1752=CARTESIAN_POINT('Ctrl Pts',(-167.796131664721,1.98940224121134,14.8691658402804));
#1753=CARTESIAN_POINT('Ctrl Pts',(-167.515408132377,2.1817038655086,14.8410532029514));
#1754=CARTESIAN_POINT('Ctrl Pts',(-166.899638702422,2.43701842756377,14.8012713411856));
#1755=CARTESIAN_POINT('Ctrl Pts',(-166.564541354955,2.5,14.790199457753));
#1756=CARTESIAN_POINT('Ctrl Pts',(-166.25,2.5,14.790199457753));
#1757=CARTESIAN_POINT('Ctrl Pts',(-165.935458645045,2.5,14.790199457753));
#1758=CARTESIAN_POINT('Ctrl Pts',(-165.600361297578,2.43701842756377,14.8012713411856));
#1759=CARTESIAN_POINT('Ctrl Pts',(-164.984591867623,2.1817038655086,14.8410532029514));
#1760=CARTESIAN_POINT('Ctrl Pts',(-164.703868335279,1.98940224121134,14.8691658402804));
#1761=CARTESIAN_POINT('Ctrl Pts',(-164.260603678422,1.54613758435443,14.9217716767288));
#1762=CARTESIAN_POINT('Ctrl Pts',(-164.068297410941,1.26541151060516,14.9497129490472));
#1763=CARTESIAN_POINT('Ctrl Pts',(-163.8129794775,0.649633350162396,14.9891013758676));
#1764=CARTESIAN_POINT('Ctrl Pts',(-163.75,0.314532953903509,15.000000000004));
#1765=CARTESIAN_POINT('Ctrl Pts',(-163.75,2.91433543964104E-15,15.000000000004));
#1766=CARTESIAN_POINT('Origin',(12.5,0.,4.44089209850063E-13));
#1767=CARTESIAN_POINT('',(0.,-3.10498508476831E-15,-24.9999999999995));
#1768=CARTESIAN_POINT('Origin',(0.,0.,0.));
#1769=CARTESIAN_POINT('',(12.5,-3.1049850847678E-15,-24.9999999999995));
#1770=CARTESIAN_POINT('Origin',(-172.5,0.,3.99680288865056E-12));
#1771=CARTESIAN_POINT('',(0.,-1.81094934657423E-15,15.000000000004));
#1772=CARTESIAN_POINT('Origin',(0.,0.,0.));
#1773=CARTESIAN_POINT('',(-172.5,-1.81094934658138E-15,15.000000000004));
#1774=CARTESIAN_POINT('',(-172.5,-1.81094934658138E-15,15.000000000004));
#1775=CARTESIAN_POINT('',(-172.5,-1.81094934658138E-15,15.000000000004));
#1776=CARTESIAN_POINT('Origin',(-172.5,0.,3.99680288865056E-12));
#1777=CARTESIAN_POINT('Origin',(12.5,0.,4.44089209850063E-13));
#1778=CARTESIAN_POINT('Origin',(0.,0.,0.));
#1779=CARTESIAN_POINT('Origin',(-172.5,0.,3.99680288865056E-12));
#1780=CARTESIAN_POINT('',(0.,0.,0.));
#1781=CARTESIAN_POINT('Origin',(-1.73472347597681E-15,-25.0000000000004,
6.24999999999996));
#1782=CARTESIAN_POINT('',(-1.42856179559609E-15,-25.0000000000024,3.74999999999996));
#1783=CARTESIAN_POINT('Ctrl Pts',(2.49999999999999,-24.8746859276679,6.24999999999996));
#1784=CARTESIAN_POINT('Ctrl Pts',(2.49999999999999,-24.8746859276679,5.93586848164138));
#1785=CARTESIAN_POINT('Ctrl Pts',(2.43717772293527,-24.8812496993573,5.6009428544044));
#1786=CARTESIAN_POINT('Ctrl Pts',(2.18197846805795,-24.9049270576873,4.98505712385862));
#1787=CARTESIAN_POINT('Ctrl Pts',(1.98961295362016,-24.9216954330504,4.7040790476874));
#1788=CARTESIAN_POINT('Ctrl Pts',(1.54592170742258,-24.9531478715761,4.26038780148982));
#1789=CARTESIAN_POINT('Ctrl Pts',(1.26494330018359,-24.9698795904327,4.06802169783962));
#1790=CARTESIAN_POINT('Ctrl Pts',(0.649056460774728,-24.9934730284172,3.81282200311052));
#1791=CARTESIAN_POINT('Ctrl Pts',(0.314130449131038,-25.0000000000024,3.74999999999997));
#1792=CARTESIAN_POINT('Ctrl Pts',(-0.314130449131041,-25.0000000000024,
3.74999999999997));
#1793=CARTESIAN_POINT('Ctrl Pts',(-0.649056460774731,-24.9934730284172,
3.81282200311052));
#1794=CARTESIAN_POINT('Ctrl Pts',(-1.26494330018359,-24.9698795904327,4.06802169783962));
#1795=CARTESIAN_POINT('Ctrl Pts',(-1.54592170742258,-24.9531478715761,4.26038780148982));
#1796=CARTESIAN_POINT('Ctrl Pts',(-1.98961295362016,-24.9216954330504,4.7040790476874));
#1797=CARTESIAN_POINT('Ctrl Pts',(-2.18197846805795,-24.9049270576873,4.98505712385862));
#1798=CARTESIAN_POINT('Ctrl Pts',(-2.43717772293527,-24.8812496993573,5.6009428544044));
#1799=CARTESIAN_POINT('Ctrl Pts',(-2.49999999999999,-24.8746859276679,5.93586848164138));
#1800=CARTESIAN_POINT('Ctrl Pts',(-2.49999999999999,-24.8746859276679,6.56413151835855));
#1801=CARTESIAN_POINT('Ctrl Pts',(-2.43717772293527,-24.8812496993573,6.89905714559553));
#1802=CARTESIAN_POINT('Ctrl Pts',(-2.18197846805795,-24.9049270576873,7.51494287614131));
#1803=CARTESIAN_POINT('Ctrl Pts',(-1.98961295362016,-24.9216954330504,7.79592095231253));
#1804=CARTESIAN_POINT('Ctrl Pts',(-1.54592170742258,-24.9531478715761,8.23961219851011));
#1805=CARTESIAN_POINT('Ctrl Pts',(-1.26494330018359,-24.9698795904327,8.43197830216031));
#1806=CARTESIAN_POINT('Ctrl Pts',(-0.649056460774732,-24.9934730284172,
8.68717799688941));
#1807=CARTESIAN_POINT('Ctrl Pts',(-0.314130449131042,-25.0000000000024,
8.74999999999996));
#1808=CARTESIAN_POINT('Ctrl Pts',(0.314130449131037,-25.0000000000024,8.74999999999996));
#1809=CARTESIAN_POINT('Ctrl Pts',(0.649056460774726,-24.9934730284172,8.68717799688941));
#1810=CARTESIAN_POINT('Ctrl Pts',(1.26494330018359,-24.9698795904327,8.43197830216031));
#1811=CARTESIAN_POINT('Ctrl Pts',(1.54592170742258,-24.9531478715761,8.23961219851011));
#1812=CARTESIAN_POINT('Ctrl Pts',(1.98961295362015,-24.9216954330504,7.79592095231254));
#1813=CARTESIAN_POINT('Ctrl Pts',(2.18197846805795,-24.9049270576873,7.51494287614131));
#1814=CARTESIAN_POINT('Ctrl Pts',(2.43717772293527,-24.8812496993573,6.89905714559553));
#1815=CARTESIAN_POINT('Ctrl Pts',(2.49999999999999,-24.8746859276679,6.56413151835855));
#1816=CARTESIAN_POINT('Ctrl Pts',(2.49999999999999,-24.8746859276679,6.24999999999996));
#1817=CARTESIAN_POINT('',(-2.15668646464658E-15,-15.0000000000024,3.74999999999997));
#1818=CARTESIAN_POINT('',(-2.04088517576354E-15,-25.0000000000004,3.74999999999997));
#1819=CARTESIAN_POINT('',(-1.73472347597681E-15,-14.9999999999981,8.74999999999997));
#1820=CARTESIAN_POINT('Ctrl Pts',(-2.22044604925031E-15,-15.0000000000024,
3.74999999999997));
#1821=CARTESIAN_POINT('Ctrl Pts',(-0.314532953903508,-15.0000000000024,
3.74999999999997));
#1822=CARTESIAN_POINT('Ctrl Pts',(-0.6496333501624,-14.989101375866,3.81297947750021));
#1823=CARTESIAN_POINT('Ctrl Pts',(-1.26541151060516,-14.9497129490456,4.0682974109409));
#1824=CARTESIAN_POINT('Ctrl Pts',(-1.54613758435442,-14.9217716767272,4.26060367842166));
#1825=CARTESIAN_POINT('Ctrl Pts',(-1.98940224121133,-14.8691658402789,4.70386833527857));
#1826=CARTESIAN_POINT('Ctrl Pts',(-2.18170386550859,-14.8410532029498,4.98459186762255));
#1827=CARTESIAN_POINT('Ctrl Pts',(-2.43701842756376,-14.8012713411841,5.60036129757765));
#1828=CARTESIAN_POINT('Ctrl Pts',(-2.49999999999999,-14.7901994577515,5.93545864504531));
#1829=CARTESIAN_POINT('Ctrl Pts',(-2.49999999999999,-14.7901994577515,6.56454135495462));
#1830=CARTESIAN_POINT('Ctrl Pts',(-2.43701842756376,-14.8012713411841,6.89963870242228));
#1831=CARTESIAN_POINT('Ctrl Pts',(-2.18170386550859,-14.8410532029498,7.51540813237737));
#1832=CARTESIAN_POINT('Ctrl Pts',(-1.98940224121133,-14.8691658402789,7.79613166472136));
#1833=CARTESIAN_POINT('Ctrl Pts',(-1.54613758435442,-14.9217716767272,8.23939632157827));
#1834=CARTESIAN_POINT('Ctrl Pts',(-1.26541151060516,-14.9497129490456,8.43170258905903));
#1835=CARTESIAN_POINT('Ctrl Pts',(-0.6496333501624,-14.989101375866,8.68702052249972));
#1836=CARTESIAN_POINT('Ctrl Pts',(-0.314532953903508,-15.0000000000024,
8.74999999999996));
#1837=CARTESIAN_POINT('Ctrl Pts',(-1.80411241501588E-15,-15.0000000000024,
8.74999999999996));
#1838=CARTESIAN_POINT('Ctrl Pts',(-1.80411241501588E-15,-15.0000000000024,
8.74999999999996));
#1839=CARTESIAN_POINT('Ctrl Pts',(0.314532953903504,-15.0000000000024,8.74999999999996));
#1840=CARTESIAN_POINT('Ctrl Pts',(0.649633350162397,-14.989101375866,8.68702052249972));
#1841=CARTESIAN_POINT('Ctrl Pts',(1.26541151060516,-14.9497129490456,8.43170258905903));
#1842=CARTESIAN_POINT('Ctrl Pts',(1.54613758435442,-14.9217716767272,8.23939632157827));
#1843=CARTESIAN_POINT('Ctrl Pts',(1.98940224121133,-14.8691658402789,7.79613166472136));
#1844=CARTESIAN_POINT('Ctrl Pts',(2.18170386550859,-14.8410532029498,7.51540813237737));
#1845=CARTESIAN_POINT('Ctrl Pts',(2.43701842756376,-14.8012713411841,6.89963870242228));
#1846=CARTESIAN_POINT('Ctrl Pts',(2.49999999999999,-14.7901994577515,6.56454135495462));
#1847=CARTESIAN_POINT('Ctrl Pts',(2.49999999999999,-14.7901994577515,6.24999999999996));
#1848=CARTESIAN_POINT('Ctrl Pts',(2.49999999999999,-14.7901994577515,5.93545864504531));
#1849=CARTESIAN_POINT('Ctrl Pts',(2.43701842756376,-14.8012713411841,5.60036129757765));
#1850=CARTESIAN_POINT('Ctrl Pts',(2.18170386550859,-14.8410532029498,4.98459186762255));
#1851=CARTESIAN_POINT('Ctrl Pts',(1.98940224121133,-14.8691658402789,4.70386833527857));
#1852=CARTESIAN_POINT('Ctrl Pts',(1.54613758435442,-14.9217716767272,4.26060367842166));
#1853=CARTESIAN_POINT('Ctrl Pts',(1.26541151060516,-14.9497129490456,4.0682974109409));
#1854=CARTESIAN_POINT('Ctrl Pts',(0.649633350162397,-14.989101375866,3.81297947750021));
#1855=CARTESIAN_POINT('Ctrl Pts',(0.314532953903504,-15.0000000000024,3.74999999999997));
#1856=CARTESIAN_POINT('Ctrl Pts',(-2.28983498828939E-15,-15.0000000000024,
3.74999999999997));
#1857=CARTESIAN_POINT('Origin',(-1.73472347597681E-15,-25.0000000000004,
6.24999999999996));
#1858=CARTESIAN_POINT('',(-1.73472347597681E-15,15.0000000000001,8.74999999999997));
#1859=CARTESIAN_POINT('',(-1.67963750875296E-15,14.9999999999975,3.74999999999997));
#1860=CARTESIAN_POINT('Ctrl Pts',(-2.22044604925031E-15,14.9999999999975,
8.74999999999996));
#1861=CARTESIAN_POINT('Ctrl Pts',(-0.314532953903508,14.9999999999975,8.74999999999996));
#1862=CARTESIAN_POINT('Ctrl Pts',(-0.6496333501624,14.9891013758612,8.68702052249972));
#1863=CARTESIAN_POINT('Ctrl Pts',(-1.26541151060517,14.9497129490408,8.43170258905903));
#1864=CARTESIAN_POINT('Ctrl Pts',(-1.54613758435443,14.9217716767223,8.23939632157827));
#1865=CARTESIAN_POINT('Ctrl Pts',(-1.98940224121133,14.869165840274,7.79613166472136));
#1866=CARTESIAN_POINT('Ctrl Pts',(-2.18170386550859,14.841053202945,7.51540813237737));
#1867=CARTESIAN_POINT('Ctrl Pts',(-2.43701842756376,14.8012713411792,6.89963870242228));
#1868=CARTESIAN_POINT('Ctrl Pts',(-2.49999999999999,14.7901994577466,6.56454135495462));
#1869=CARTESIAN_POINT('Ctrl Pts',(-2.49999999999999,14.7901994577466,5.93545864504531));
#1870=CARTESIAN_POINT('Ctrl Pts',(-2.43701842756376,14.8012713411792,5.60036129757765));
#1871=CARTESIAN_POINT('Ctrl Pts',(-2.18170386550859,14.841053202945,4.98459186762255));
#1872=CARTESIAN_POINT('Ctrl Pts',(-1.98940224121133,14.869165840274,4.70386833527857));
#1873=CARTESIAN_POINT('Ctrl Pts',(-1.54613758435442,14.9217716767223,4.26060367842166));
#1874=CARTESIAN_POINT('Ctrl Pts',(-1.26541151060516,14.9497129490408,4.0682974109409));
#1875=CARTESIAN_POINT('Ctrl Pts',(-0.649633350162399,14.9891013758612,3.81297947750021));
#1876=CARTESIAN_POINT('Ctrl Pts',(-0.314532953903507,14.9999999999975,3.74999999999997));
#1877=CARTESIAN_POINT('Ctrl Pts',(-1.2490009027033E-15,14.9999999999975,
3.74999999999997));
#1878=CARTESIAN_POINT('',(-1.34182558298458E-15,24.9999999999976,3.74999999999996));
#1879=CARTESIAN_POINT('',(-2.04088517576354E-15,-25.0000000000004,3.74999999999997));
#1880=CARTESIAN_POINT('Ctrl Pts',(2.49999999999999,24.874685927663,6.24999999999996));
#1881=CARTESIAN_POINT('Ctrl Pts',(2.49999999999999,24.874685927663,6.56413151835855));
#1882=CARTESIAN_POINT('Ctrl Pts',(2.43717772293527,24.8812496993524,6.89905714559553));
#1883=CARTESIAN_POINT('Ctrl Pts',(2.18197846805795,24.9049270576824,7.51494287614131));
#1884=CARTESIAN_POINT('Ctrl Pts',(1.98961295362016,24.9216954330456,7.79592095231253));
#1885=CARTESIAN_POINT('Ctrl Pts',(1.54592170742258,24.9531478715712,8.23961219851011));
#1886=CARTESIAN_POINT('Ctrl Pts',(1.26494330018359,24.9698795904278,8.43197830216031));
#1887=CARTESIAN_POINT('Ctrl Pts',(0.649056460774728,24.9934730284123,8.68717799688941));
#1888=CARTESIAN_POINT('Ctrl Pts',(0.314130449131038,24.9999999999975,8.74999999999996));
#1889=CARTESIAN_POINT('Ctrl Pts',(-0.314130449131041,24.9999999999975,8.74999999999996));
#1890=CARTESIAN_POINT('Ctrl Pts',(-0.649056460774732,24.9934730284123,8.68717799688941));
#1891=CARTESIAN_POINT('Ctrl Pts',(-1.26494330018359,24.9698795904278,8.43197830216031));
#1892=CARTESIAN_POINT('Ctrl Pts',(-1.54592170742258,24.9531478715712,8.23961219851011));
#1893=CARTESIAN_POINT('Ctrl Pts',(-1.98961295362016,24.9216954330456,7.79592095231253));
#1894=CARTESIAN_POINT('Ctrl Pts',(-2.18197846805795,24.9049270576824,7.51494287614131));
#1895=CARTESIAN_POINT('Ctrl Pts',(-2.43717772293527,24.8812496993524,6.89905714559553));
#1896=CARTESIAN_POINT('Ctrl Pts',(-2.49999999999999,24.874685927663,6.56413151835855));
#1897=CARTESIAN_POINT('Ctrl Pts',(-2.49999999999999,24.874685927663,5.93586848164138));
#1898=CARTESIAN_POINT('Ctrl Pts',(-2.43717772293527,24.8812496993524,5.6009428544044));
#1899=CARTESIAN_POINT('Ctrl Pts',(-2.18197846805795,24.9049270576824,4.98505712385862));
#1900=CARTESIAN_POINT('Ctrl Pts',(-1.98961295362016,24.9216954330456,4.7040790476874));
#1901=CARTESIAN_POINT('Ctrl Pts',(-1.54592170742258,24.9531478715712,4.26038780148982));
#1902=CARTESIAN_POINT('Ctrl Pts',(-1.26494330018359,24.9698795904278,4.06802169783962));
#1903=CARTESIAN_POINT('Ctrl Pts',(-0.649056460774731,24.9934730284123,3.81282200311052));
#1904=CARTESIAN_POINT('Ctrl Pts',(-0.314130449131041,24.9999999999975,3.74999999999997));
#1905=CARTESIAN_POINT('Ctrl Pts',(0.314130449131038,24.9999999999975,3.74999999999997));
#1906=CARTESIAN_POINT('Ctrl Pts',(0.649056460774727,24.9934730284123,3.81282200311052));
#1907=CARTESIAN_POINT('Ctrl Pts',(1.26494330018359,24.9698795904278,4.06802169783962));
#1908=CARTESIAN_POINT('Ctrl Pts',(1.54592170742258,24.9531478715712,4.26038780148982));
#1909=CARTESIAN_POINT('Ctrl Pts',(1.98961295362016,24.9216954330456,4.7040790476874));
#1910=CARTESIAN_POINT('Ctrl Pts',(2.18197846805795,24.9049270576824,4.98505712385862));
#1911=CARTESIAN_POINT('Ctrl Pts',(2.43717772293527,24.8812496993524,5.6009428544044));
#1912=CARTESIAN_POINT('Ctrl Pts',(2.49999999999999,24.874685927663,5.93586848164138));
#1913=CARTESIAN_POINT('Ctrl Pts',(2.49999999999999,24.874685927663,6.24999999999996));
#1914=CARTESIAN_POINT('Ctrl Pts',(-1.31838984174237E-15,14.9999999999975,
3.74999999999997));
#1915=CARTESIAN_POINT('Ctrl Pts',(0.314532953903505,14.9999999999975,3.74999999999997));
#1916=CARTESIAN_POINT('Ctrl Pts',(0.649633350162396,14.9891013758612,3.81297947750021));
#1917=CARTESIAN_POINT('Ctrl Pts',(1.26541151060516,14.9497129490408,4.0682974109409));
#1918=CARTESIAN_POINT('Ctrl Pts',(1.54613758435442,14.9217716767223,4.26060367842166));
#1919=CARTESIAN_POINT('Ctrl Pts',(1.98940224121133,14.869165840274,4.70386833527857));
#1920=CARTESIAN_POINT('Ctrl Pts',(2.18170386550859,14.841053202945,4.98459186762255));
#1921=CARTESIAN_POINT('Ctrl Pts',(2.43701842756376,14.8012713411792,5.60036129757765));
#1922=CARTESIAN_POINT('Ctrl Pts',(2.49999999999999,14.7901994577466,5.93545864504531));
#1923=CARTESIAN_POINT('Ctrl Pts',(2.49999999999999,14.7901994577466,6.24999999999996));
#1924=CARTESIAN_POINT('Ctrl Pts',(2.49999999999999,14.7901994577466,6.56454135495462));
#1925=CARTESIAN_POINT('Ctrl Pts',(2.43701842756376,14.8012713411792,6.89963870242228));
#1926=CARTESIAN_POINT('Ctrl Pts',(2.18170386550859,14.841053202945,7.51540813237737));
#1927=CARTESIAN_POINT('Ctrl Pts',(1.98940224121133,14.869165840274,7.79613166472136));
#1928=CARTESIAN_POINT('Ctrl Pts',(1.54613758435442,14.9217716767223,8.23939632157827));
#1929=CARTESIAN_POINT('Ctrl Pts',(1.26541151060516,14.9497129490408,8.43170258905903));
#1930=CARTESIAN_POINT('Ctrl Pts',(0.649633350162395,14.9891013758612,8.68702052249972));
#1931=CARTESIAN_POINT('Ctrl Pts',(0.314532953903504,14.9999999999975,8.74999999999996));
#1932=CARTESIAN_POINT('Ctrl Pts',(-2.22044604925031E-15,14.9999999999975,
8.74999999999996));
#1933=CARTESIAN_POINT('Origin',(-1.73472347597681E-15,-2.44249065417534E-12,
12.5));
#1934=CARTESIAN_POINT('',(15.,-2.44435364522621E-12,12.5));
#1935=CARTESIAN_POINT('Origin',(-1.73472347597681E-15,-2.44249065417534E-12,
12.5));
#1936=CARTESIAN_POINT('',(15.,-2.44435364522621E-12,0.));
#1937=CARTESIAN_POINT('',(15.,-2.44435364522621E-12,12.5));
#1938=CARTESIAN_POINT('Origin',(0.,0.,0.));
#1939=CARTESIAN_POINT('Origin',(-1.73472347597681E-15,-2.44249065417534E-12,
12.5));
#1940=CARTESIAN_POINT('',(25.,-2.44559563926011E-12,2.22044604925031E-15));
#1941=CARTESIAN_POINT('Origin',(0.,0.,0.));
#1942=CARTESIAN_POINT('',(25.,-2.44559563926011E-12,12.5));
#1943=CARTESIAN_POINT('',(25.,-2.44559563926011E-12,12.5));
#1944=CARTESIAN_POINT('Origin',(-1.73472347597681E-15,-2.44249065417534E-12,
12.5));
#1945=CARTESIAN_POINT('Origin',(-1.73472347597681E-15,-2.44249065417534E-12,
12.5));
#1946=CARTESIAN_POINT('Origin',(0.,0.,0.));
#1947=CARTESIAN_POINT('',(0.,0.,0.));
#1948=CARTESIAN_POINT('Origin',(0.,-5.55111512312578E-14,60.0000000000028));
#1949=CARTESIAN_POINT('',(2.49999999999999,-1.01914783176794E-13,0.));
#1950=CARTESIAN_POINT('Origin',(0.,0.,0.));
#1951=CARTESIAN_POINT('',(2.49999999999999,-6.15072059322486E-14,60.0000000000028));
#1952=CARTESIAN_POINT('',(2.49999999999999,-6.15072059322486E-14,60.0000000000028));
#1953=CARTESIAN_POINT('Origin',(0.,-5.55111512312578E-14,60.0000000000028));
#1954=CARTESIAN_POINT('Origin',(0.,-5.55111512312578E-14,60.0000000000028));
#1955=CARTESIAN_POINT('Origin',(0.,0.,0.));
#1956=CARTESIAN_POINT('',(0.,0.,0.));
#1957=CARTESIAN_POINT('Origin',(-2.22044604925031E-13,0.,150.));
#1958=CARTESIAN_POINT('',(-10.0000000000013,22.9128784747792,-8.88178419700125E-13));
#1959=CARTESIAN_POINT('',(24.9999999999999,-3.06161699786961E-15,-8.88178419700125E-13));
#1960=CARTESIAN_POINT('Origin',(0.,0.,0.));
#1961=CARTESIAN_POINT('',(24.9999999999999,-3.06161699786845E-15,150.));
#1962=CARTESIAN_POINT('',(24.9999999999999,-3.06161699786845E-15,150.));
#1963=CARTESIAN_POINT('Origin',(-2.22044604925031E-13,0.,150.));
#1964=CARTESIAN_POINT('',(10.,22.9128784747792,0.));
#1965=CARTESIAN_POINT('Origin',(0.,0.,0.));
#1966=CARTESIAN_POINT('',(9.99999999999912,22.9128784747793,89.7797711496207));
#1967=CARTESIAN_POINT('',(9.99999999999979,22.9128784747792,150.));
#1968=CARTESIAN_POINT('',(-10.000000000001,22.9128784747793,89.7797711496216));
#1969=CARTESIAN_POINT('Ctrl Pts',(9.99999999999965,22.9128784747794,89.7797711496257));
#1970=CARTESIAN_POINT('Ctrl Pts',(8.91671999216883,23.3856606304668,89.8806685836023));
#1971=CARTESIAN_POINT('Ctrl Pts',(7.77197604014579,23.792186686818,89.9320009552562));
#1972=CARTESIAN_POINT('Ctrl Pts',(5.50330393661502,24.4133362342407,89.9873423916812));
#1973=CARTESIAN_POINT('Ctrl Pts',(4.3815649951061,24.6385720078244,89.9945429930909));
#1974=CARTESIAN_POINT('Ctrl Pts',(2.15820493465309,24.9318971171076,90.0008440556194));
#1975=CARTESIAN_POINT('Ctrl Pts',(1.05658576058149,25.0000000000002,90.0000000000046));
#1976=CARTESIAN_POINT('Ctrl Pts',(-1.05658576058194,25.0000000000002,90.0000000000046));
#1977=CARTESIAN_POINT('Ctrl Pts',(-2.15820493465353,24.9318971171076,90.0008440556194));
#1978=CARTESIAN_POINT('Ctrl Pts',(-4.38156499510654,24.6385720078244,89.9945429930909));
#1979=CARTESIAN_POINT('Ctrl Pts',(-5.50330393661546,24.4133362342407,89.9873423916812));
#1980=CARTESIAN_POINT('Ctrl Pts',(-7.77197604014664,23.7921866868179,89.9320009552562));
#1981=CARTESIAN_POINT('Ctrl Pts',(-8.91671999217008,23.3856606304665,89.8806685836023));
#1982=CARTESIAN_POINT('Ctrl Pts',(-10.0000000000012,22.9128784747789,89.7797711496256));
#1983=CARTESIAN_POINT('',(-10.,22.9128784747792,150.));
#1984=CARTESIAN_POINT('Origin',(0.,0.,0.));
#1985=CARTESIAN_POINT('',(-10.0000000000013,15.,-8.88178419700125E-13));
#1986=CARTESIAN_POINT('',(-10.0000000000013,0.,-8.88178419700125E-13));
#1987=CARTESIAN_POINT('',(10.,15.,0.));
#1988=CARTESIAN_POINT('',(-10.0000000000013,15.,-8.88178419700125E-13));
#1989=CARTESIAN_POINT('',(10.,15.,0.));
#1990=CARTESIAN_POINT('Origin',(-2.22044604925031E-13,0.,150.));
#1991=CARTESIAN_POINT('Origin',(-10.0000000000002,27.1241010986052,90.0000000000003));
#1992=CARTESIAN_POINT('',(-10.0000000000009,15.0000000000003,80.0000000000041));
#1993=CARTESIAN_POINT('Origin',(-10.000000000001,25.,80.0000000000045));
#1994=CARTESIAN_POINT('',(-10.0000000000002,15.,90.0000000000003));
#1995=CARTESIAN_POINT('Origin',(9.99999999999979,15.,89.9999999999994));
#1996=CARTESIAN_POINT('',(9.99999999999945,15.,80.0000000000036));
#1997=CARTESIAN_POINT('',(9.99999999999979,15.,89.9999999999994));
#1998=CARTESIAN_POINT('Origin',(9.99999999999934,25.,80.0000000000036));
#1999=CARTESIAN_POINT('Origin',(-10.0000000000002,15.,90.0000000000003));
#2000=CARTESIAN_POINT('',(-10.0000000000009,15.0000000000003,80.0000000000041));
#2001=CARTESIAN_POINT('Origin',(-10.000000000001,25.,80.0000000000045));
#2002=CARTESIAN_POINT('',(0.,0.,0.));
#2003=CARTESIAN_POINT('Origin',(9.99200722162641E-13,-1.11022302462516E-13,
80.0000000000001));
#2004=CARTESIAN_POINT('',(-5.55111512312578E-14,20.,70.0000000000016));
#2005=CARTESIAN_POINT('',(9.99200722162641E-13,20.,9.9999999999969));
#2006=CARTESIAN_POINT('',(9.99200722162641E-13,19.9999999999999,80.0000000000001));
#2007=CARTESIAN_POINT('',(9.99200722162641E-13,0.,9.9999999999969));
#2008=CARTESIAN_POINT('',(9.99200722162641E-13,0.,9.9999999999969));
#2009=CARTESIAN_POINT('',(-5.55111512312578E-14,0.,70.0000000000016));
#2010=CARTESIAN_POINT('',(9.99200722162641E-13,-1.11022302462516E-13,80.0000000000001));
#2011=CARTESIAN_POINT('',(-5.55111512312578E-14,0.,70.0000000000016));
#2012=CARTESIAN_POINT('Origin',(9.99200722162641E-13,-1.11022302462516E-13,
80.0000000000001));
#2013=CARTESIAN_POINT('',(20.0000000000001,0.,10.0000000000002));
#2014=CARTESIAN_POINT('Origin',(10.0000000000001,0.,10.0000000000002));
#2015=CARTESIAN_POINT('',(20.000000000001,-1.11022302462516E-13,69.9999999999994));
#2016=CARTESIAN_POINT('',(20.0000000000001,-1.11022302462516E-13,80.0000000000003));
#2017=CARTESIAN_POINT('Origin',(10.000000000001,0.,70.0000000000005));
#2018=CARTESIAN_POINT('Origin',(20.0000000000001,-1.11022302462516E-13,
80.0000000000003));
#2019=CARTESIAN_POINT('',(20.0000000000001,20.,10.0000000000002));
#2020=CARTESIAN_POINT('',(20.0000000000001,20.,10.0000000000002));
#2021=CARTESIAN_POINT('',(20.000000000001,19.9999999999999,69.9999999999994));
#2022=CARTESIAN_POINT('',(20.0000000000001,19.9999999999999,80.0000000000003));
#2023=CARTESIAN_POINT('',(20.000000000001,-1.11022302462516E-13,69.9999999999994));
#2024=CARTESIAN_POINT('Origin',(9.99200722162641E-13,19.9999999999999,80.0000000000001));
#2025=CARTESIAN_POINT('Origin',(10.0000000000001,20.,10.0000000000002));
#2026=CARTESIAN_POINT('Origin',(10.000000000001,20.,70.0000000000005));
#2027=CARTESIAN_POINT('Origin',(10.0000000000001,0.,10.0000000000002));
#2028=CARTESIAN_POINT('Origin',(10.000000000001,0.,70.0000000000005));
#2029=CARTESIAN_POINT('',(25.1465973098743,-2.7881296588248,-55.8215751054195));
#2030=CARTESIAN_POINT('',(-74.9279377599,24.835204097004,-1.78266675396573));
#2031=CARTESIAN_POINT('',(25.1465973098745,-2.78812965882478,79.1784248945814));
#2032=CARTESIAN_POINT('',(25.1465973098743,-2.78812965882481,-93.3215751054186));
#2033=CARTESIAN_POINT('',(0.14692655133643,-2.91643384701778,-87.0715751054194));
#2034=CARTESIAN_POINT('',(-84.8444462906221,-2.78812965882476,-1.94131423281088));
#2035=CARTESIAN_POINT('',(-84.6844835581376,12.2118703411752,-11.9400347471675));
#2036=CARTESIAN_POINT('',(85.2287684850808,-2.86666551003765,-28.4449088612482));
#2037=CARTESIAN_POINT('',(-14.8534026901257,-82.7881296588248,-0.82157510541947));
#2038=CARTESIAN_POINT('',(-14.8534026901257,89.7118703411752,-0.82157510541947));
#2039=CARTESIAN_POINT('',(-14.8534026901257,83.4618703411752,-25.8215751054195));
#2040=CARTESIAN_POINT('',(95.1465375083653,-2.87962942956916,-0.821575105419373));
#2041=CARTESIAN_POINT('',(95.1334661125448,-12.8796208864954,-35.8215751054193));
#2042=UNCERTAINTY_MEASURE_WITH_UNIT(LENGTH_MEASURE(0.01),#2060,
'DISTANCE_ACCURACY_VALUE',
'Maximum model space distance between geometric entities at asserted c
onnectivities');
#2043=UNCERTAINTY_MEASURE_WITH_UNIT(LENGTH_MEASURE(0.01),#2060,
'DISTANCE_ACCURACY_VALUE',
'Maximum model space distance between geometric entities at asserted c
onnectivities');
#2044=UNCERTAINTY_MEASURE_WITH_UNIT(LENGTH_MEASURE(0.01),#2060,
'DISTANCE_ACCURACY_VALUE',
'Maximum model space distance between geometric entities at asserted c
onnectivities');
#2045=UNCERTAINTY_MEASURE_WITH_UNIT(LENGTH_MEASURE(0.01),#2060,
'DISTANCE_ACCURACY_VALUE',
'Maximum model space distance between geometric entities at asserted c
onnectivities');
#2046=UNCERTAINTY_MEASURE_WITH_UNIT(LENGTH_MEASURE(0.01),#2060,
'DISTANCE_ACCURACY_VALUE',
'Maximum model space distance between geometric entities at asserted c
onnectivities');
#2047=UNCERTAINTY_MEASURE_WITH_UNIT(LENGTH_MEASURE(0.01),#2060,
'DISTANCE_ACCURACY_VALUE',
'Maximum model space distance between geometric entities at asserted c
onnectivities');
#2048=UNCERTAINTY_MEASURE_WITH_UNIT(LENGTH_MEASURE(0.01),#2060,
'DISTANCE_ACCURACY_VALUE',
'Maximum model space distance between geometric entities at asserted c
onnectivities');
#2049=UNCERTAINTY_MEASURE_WITH_UNIT(LENGTH_MEASURE(0.01),#2060,
'DISTANCE_ACCURACY_VALUE',
'Maximum model space distance between geometric entities at asserted c
onnectivities');
#2050=UNCERTAINTY_MEASURE_WITH_UNIT(LENGTH_MEASURE(0.01),#2060,
'DISTANCE_ACCURACY_VALUE',
'Maximum model space distance between geometric entities at asserted c
onnectivities');
#2051=(
GEOMETRIC_REPRESENTATION_CONTEXT(3)
GLOBAL_UNCERTAINTY_ASSIGNED_CONTEXT((#2042))
GLOBAL_UNIT_ASSIGNED_CONTEXT((#2060,#2062,#2063))
REPRESENTATION_CONTEXT('','3D')
);
#2052=(
GEOMETRIC_REPRESENTATION_CONTEXT(3)
GLOBAL_UNCERTAINTY_ASSIGNED_CONTEXT((#2043))
GLOBAL_UNIT_ASSIGNED_CONTEXT((#2060,#2062,#2063))
REPRESENTATION_CONTEXT('','3D')
);
#2053=(
GEOMETRIC_REPRESENTATION_CONTEXT(3)
GLOBAL_UNCERTAINTY_ASSIGNED_CONTEXT((#2044))
GLOBAL_UNIT_ASSIGNED_CONTEXT((#2060,#2062,#2063))
REPRESENTATION_CONTEXT('','3D')
);
#2054=(
GEOMETRIC_REPRESENTATION_CONTEXT(3)
GLOBAL_UNCERTAINTY_ASSIGNED_CONTEXT((#2045))
GLOBAL_UNIT_ASSIGNED_CONTEXT((#2060,#2062,#2063))
REPRESENTATION_CONTEXT('','3D')
);
#2055=(
GEOMETRIC_REPRESENTATION_CONTEXT(3)
GLOBAL_UNCERTAINTY_ASSIGNED_CONTEXT((#2046))
GLOBAL_UNIT_ASSIGNED_CONTEXT((#2060,#2062,#2063))
REPRESENTATION_CONTEXT('','3D')
);
#2056=(
GEOMETRIC_REPRESENTATION_CONTEXT(3)
GLOBAL_UNCERTAINTY_ASSIGNED_CONTEXT((#2047))
GLOBAL_UNIT_ASSIGNED_CONTEXT((#2060,#2062,#2063))
REPRESENTATION_CONTEXT('','3D')
);
#2057=(
GEOMETRIC_REPRESENTATION_CONTEXT(3)
GLOBAL_UNCERTAINTY_ASSIGNED_CONTEXT((#2048))
GLOBAL_UNIT_ASSIGNED_CONTEXT((#2060,#2062,#2063))
REPRESENTATION_CONTEXT('','3D')
);
#2058=(
GEOMETRIC_REPRESENTATION_CONTEXT(3)
GLOBAL_UNCERTAINTY_ASSIGNED_CONTEXT((#2049))
GLOBAL_UNIT_ASSIGNED_CONTEXT((#2060,#2062,#2063))
REPRESENTATION_CONTEXT('','3D')
);
#2059=(
GEOMETRIC_REPRESENTATION_CONTEXT(3)
GLOBAL_UNCERTAINTY_ASSIGNED_CONTEXT((#2050))
GLOBAL_UNIT_ASSIGNED_CONTEXT((#2060,#2062,#2063))
REPRESENTATION_CONTEXT('','3D')
);
#2060=(
LENGTH_UNIT()
NAMED_UNIT(*)
SI_UNIT(.MILLI.,.METRE.)
);
#2061=(
LENGTH_UNIT()
NAMED_UNIT(*)
SI_UNIT($,.METRE.)
);
#2062=(
NAMED_UNIT(*)
PLANE_ANGLE_UNIT()
SI_UNIT($,.RADIAN.)
);
#2063=(
NAMED_UNIT(*)
SI_UNIT($,.STERADIAN.)
SOLID_ANGLE_UNIT()
);
#2064=SHAPE_DEFINITION_REPRESENTATION(#2072,#2093);
#2065=SHAPE_DEFINITION_REPRESENTATION(#2073,#2094);
#2066=SHAPE_DEFINITION_REPRESENTATION(#2074,#2095);
#2067=SHAPE_DEFINITION_REPRESENTATION(#2075,#2096);
#2068=SHAPE_DEFINITION_REPRESENTATION(#2076,#2097);
#2069=SHAPE_DEFINITION_REPRESENTATION(#2077,#2098);
#2070=SHAPE_DEFINITION_REPRESENTATION(#2078,#2099);
#2071=SHAPE_DEFINITION_REPRESENTATION(#2079,#2100);
#2072=PRODUCT_DEFINITION_SHAPE('',$,#2102);
#2073=PRODUCT_DEFINITION_SHAPE('',$,#2103);
#2074=PRODUCT_DEFINITION_SHAPE('',$,#2104);
#2075=PRODUCT_DEFINITION_SHAPE('',$,#2105);
#2076=PRODUCT_DEFINITION_SHAPE('',$,#2106);
#2077=PRODUCT_DEFINITION_SHAPE('',$,#2107);
#2078=PRODUCT_DEFINITION_SHAPE('',$,#2108);
#2079=PRODUCT_DEFINITION_SHAPE('',$,#2109);
#2080=PRODUCT_DEFINITION_SHAPE($,$,#50);
#2081=PRODUCT_DEFINITION_SHAPE($,$,#51);
#2082=PRODUCT_DEFINITION_SHAPE($,$,#52);
#2083=PRODUCT_DEFINITION_SHAPE($,$,#53);
#2084=PRODUCT_DEFINITION_SHAPE($,$,#54);
#2085=PRODUCT_DEFINITION_SHAPE($,$,#55);
#2086=PRODUCT_DEFINITION_SHAPE($,$,#56);
#2087=PRODUCT_DEFINITION_SHAPE($,$,#57);
#2088=PRODUCT_DEFINITION_SHAPE($,$,#58);
#2089=PRODUCT_DEFINITION_SHAPE($,$,#59);
#2090=PRODUCT_DEFINITION_SHAPE($,$,#60);
#2091=PRODUCT_DEFINITION_SHAPE($,$,#61);
#2092=PRODUCT_DEFINITION_SHAPE($,$,#62);
#2093=SHAPE_REPRESENTATION('',(#1060,#1167,#1168,#1169,#1170,#1171,#1172,
#1173,#1174,#1175,#1176,#1177,#1178,#1179),#2051);
#2094=SHAPE_REPRESENTATION('',(#1061),#2052);
#2095=SHAPE_REPRESENTATION('',(#1078),#2053);
#2096=SHAPE_REPRESENTATION('',(#1111),#2054);
#2097=SHAPE_REPRESENTATION('',(#1126),#2055);
#2098=SHAPE_REPRESENTATION('',(#1137),#2056);
#2099=SHAPE_REPRESENTATION('',(#1143),#2057);
#2100=SHAPE_REPRESENTATION('',(#1156),#2058);
#2101=PRODUCT_DEFINITION_CONTEXT('part definition',#2127,'design');
#2102=PRODUCT_DEFINITION('MAT-037','MAT-037',#2110,#2101);
#2103=PRODUCT_DEFINITION('interconnect','interconnect',#2111,#2101);
#2104=PRODUCT_DEFINITION('hooks','hooks',#2112,#2101);
#2105=PRODUCT_DEFINITION('bolt','bolt',#2113,#2101);
#2106=PRODUCT_DEFINITION('Ring','ring',#2114,#2101);
#2107=PRODUCT_DEFINITION('Pin','PIN',#2115,#2101);
#2108=PRODUCT_DEFINITION('Shaft','shaft',#2116,#2101);
#2109=PRODUCT_DEFINITION('keu','key',#2117,#2101);
#2110=PRODUCT_DEFINITION_FORMATION('',$,#2129);
#2111=PRODUCT_DEFINITION_FORMATION('',$,#2130);
#2112=PRODUCT_DEFINITION_FORMATION('',$,#2131);
#2113=PRODUCT_DEFINITION_FORMATION('',$,#2132);
#2114=PRODUCT_DEFINITION_FORMATION('',$,#2133);
#2115=PRODUCT_DEFINITION_FORMATION('',$,#2134);
#2116=PRODUCT_DEFINITION_FORMATION('',$,#2135);
#2117=PRODUCT_DEFINITION_FORMATION('',$,#2136);
#2118=PRODUCT_RELATED_PRODUCT_CATEGORY('MAT-037','MAT-037',(#2129));
#2119=PRODUCT_RELATED_PRODUCT_CATEGORY('interconnect','interconnect',(#2130));
#2120=PRODUCT_RELATED_PRODUCT_CATEGORY('hooks','hooks',(#2131));
#2121=PRODUCT_RELATED_PRODUCT_CATEGORY('bolt','bolt',(#2132));
#2122=PRODUCT_RELATED_PRODUCT_CATEGORY('ring','ring',(#2133));
#2123=PRODUCT_RELATED_PRODUCT_CATEGORY('PIN','PIN',(#2134));
#2124=PRODUCT_RELATED_PRODUCT_CATEGORY('shaft','shaft',(#2135));
#2125=PRODUCT_RELATED_PRODUCT_CATEGORY('key','key',(#2136));
#2126=APPLICATION_PROTOCOL_DEFINITION('international standard',
'automotive_design',2009,#2127);
#2127=APPLICATION_CONTEXT(
'Core Data for Automotive Mechanical Design Process');
#2128=PRODUCT_CONTEXT('part definition',#2127,'mechanical');
#2129=PRODUCT('MAT-037','MAT-037','STEP AP214',(#2128));
#2130=PRODUCT('interconnect','interconnect',$,(#2128));
#2131=PRODUCT('hooks','hooks',$,(#2128));
#2132=PRODUCT('bolt','bolt',$,(#2128));
#2133=PRODUCT('Ring','ring',$,(#2128));
#2134=PRODUCT('Pin','PIN',$,(#2128));
#2135=PRODUCT('Shaft','shaft','Shaft',(#2128));
#2136=PRODUCT('keu','key',$,(#2128));
#2137=PRESENTATION_STYLE_ASSIGNMENT((#2143));
#2138=PRESENTATION_STYLE_ASSIGNMENT((#2144));
#2139=PRESENTATION_STYLE_ASSIGNMENT((#2145));
#2140=PRESENTATION_STYLE_ASSIGNMENT((#2146));
#2141=PRESENTATION_STYLE_ASSIGNMENT((#2147));
#2142=PRESENTATION_STYLE_ASSIGNMENT((#2148));
#2143=SURFACE_STYLE_USAGE(.BOTH.,#2149);
#2144=SURFACE_STYLE_USAGE(.BOTH.,#2150);
#2145=SURFACE_STYLE_USAGE(.BOTH.,#2151);
#2146=SURFACE_STYLE_USAGE(.BOTH.,#2152);
#2147=SURFACE_STYLE_USAGE(.BOTH.,#2153);
#2148=SURFACE_STYLE_USAGE(.BOTH.,#2154);
#2149=SURFACE_SIDE_STYLE('',(#2155));
#2150=SURFACE_SIDE_STYLE('',(#2156));
#2151=SURFACE_SIDE_STYLE('',(#2157));
#2152=SURFACE_SIDE_STYLE('',(#2158));
#2153=SURFACE_SIDE_STYLE('',(#2159));
#2154=SURFACE_SIDE_STYLE('',(#2160));
#2155=SURFACE_STYLE_FILL_AREA(#2161);
#2156=SURFACE_STYLE_FILL_AREA(#2162);
#2157=SURFACE_STYLE_FILL_AREA(#2163);
#2158=SURFACE_STYLE_FILL_AREA(#2164);
#2159=SURFACE_STYLE_FILL_AREA(#2165);
#2160=SURFACE_STYLE_FILL_AREA(#2166);
#2161=FILL_AREA_STYLE('Steel - Satin',(#2167));
#2162=FILL_AREA_STYLE('Opaque(227,224,212)',(#2168));
#2163=FILL_AREA_STYLE('Opaque(61,176,222)',(#2169));
#2164=FILL_AREA_STYLE('Opaque(31,36,43)',(#2170));
#2165=FILL_AREA_STYLE('Opaque(97,158,199)',(#2171));
#2166=FILL_AREA_STYLE('Opaque(122,133,145)',(#2172));
#2167=FILL_AREA_STYLE_COLOUR('Steel - Satin',#2173);
#2168=FILL_AREA_STYLE_COLOUR('Opaque(227,224,212)',#2174);
#2169=FILL_AREA_STYLE_COLOUR('Opaque(61,176,222)',#2175);
#2170=FILL_AREA_STYLE_COLOUR('Opaque(31,36,43)',#2176);
#2171=FILL_AREA_STYLE_COLOUR('Opaque(97,158,199)',#2177);
#2172=FILL_AREA_STYLE_COLOUR('Opaque(122,133,145)',#2178);
#2173=COLOUR_RGB('Steel - Satin',0.627450980392157,0.627450980392157,0.627450980392157);
#2174=COLOUR_RGB('Opaque(227,224,212)',0.890196078431372,0.87843137254902,
0.831372549019608);
#2175=COLOUR_RGB('Opaque(61,176,222)',0.23921568627451,0.690196078431373,
0.870588235294118);
#2176=COLOUR_RGB('Opaque(31,36,43)',0.12156862745098,0.141176470588235,
0.168627450980392);
#2177=COLOUR_RGB('Opaque(97,158,199)',0.380392156862745,0.619607843137255,
0.780392156862745);
#2178=COLOUR_RGB('Opaque(122,133,145)',0.47843137254902,0.52156862745098,
0.568627450980392);
ENDSEC;
END-ISO-10303-21;
